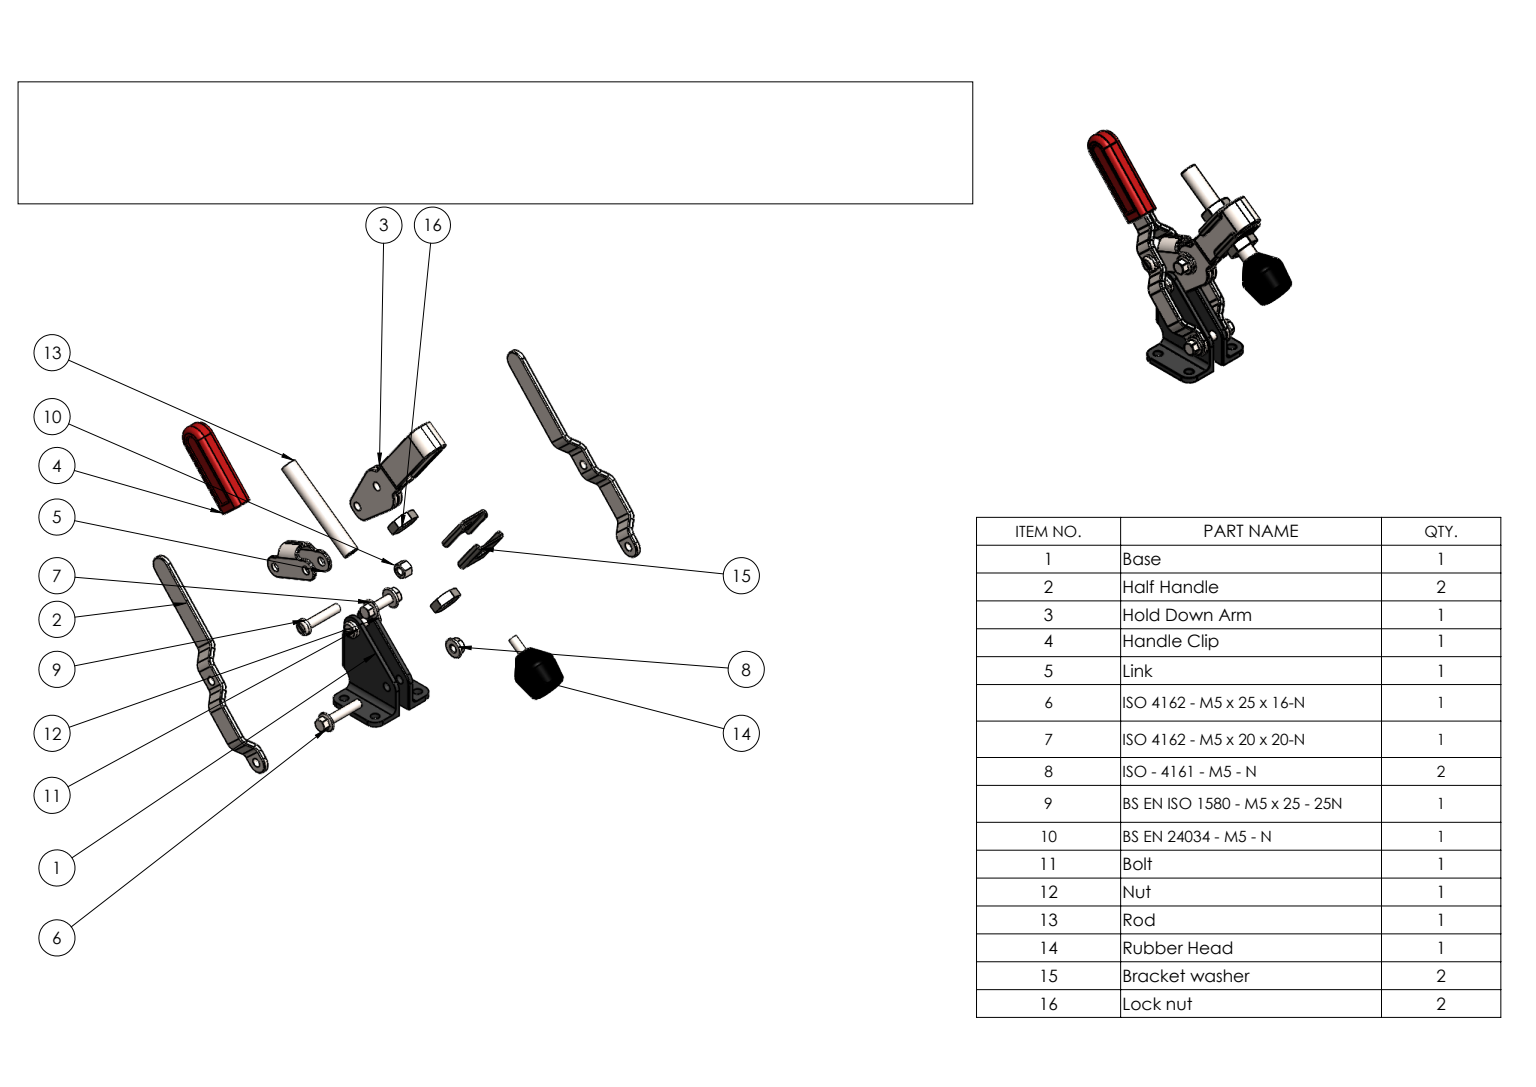
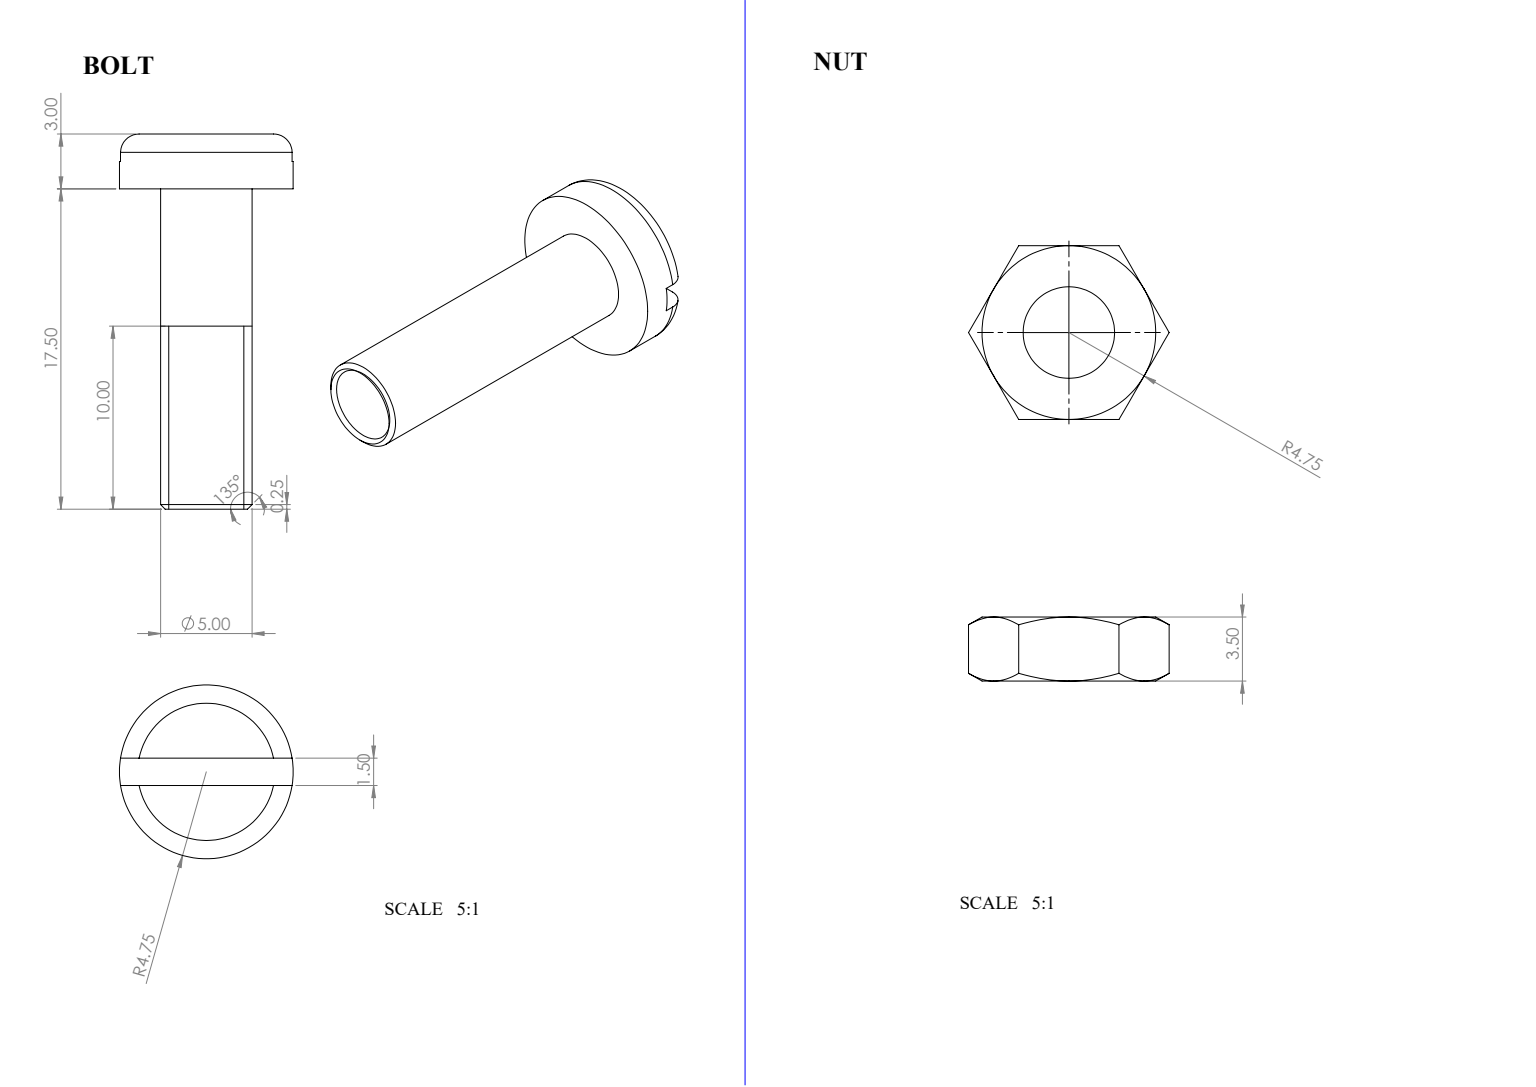
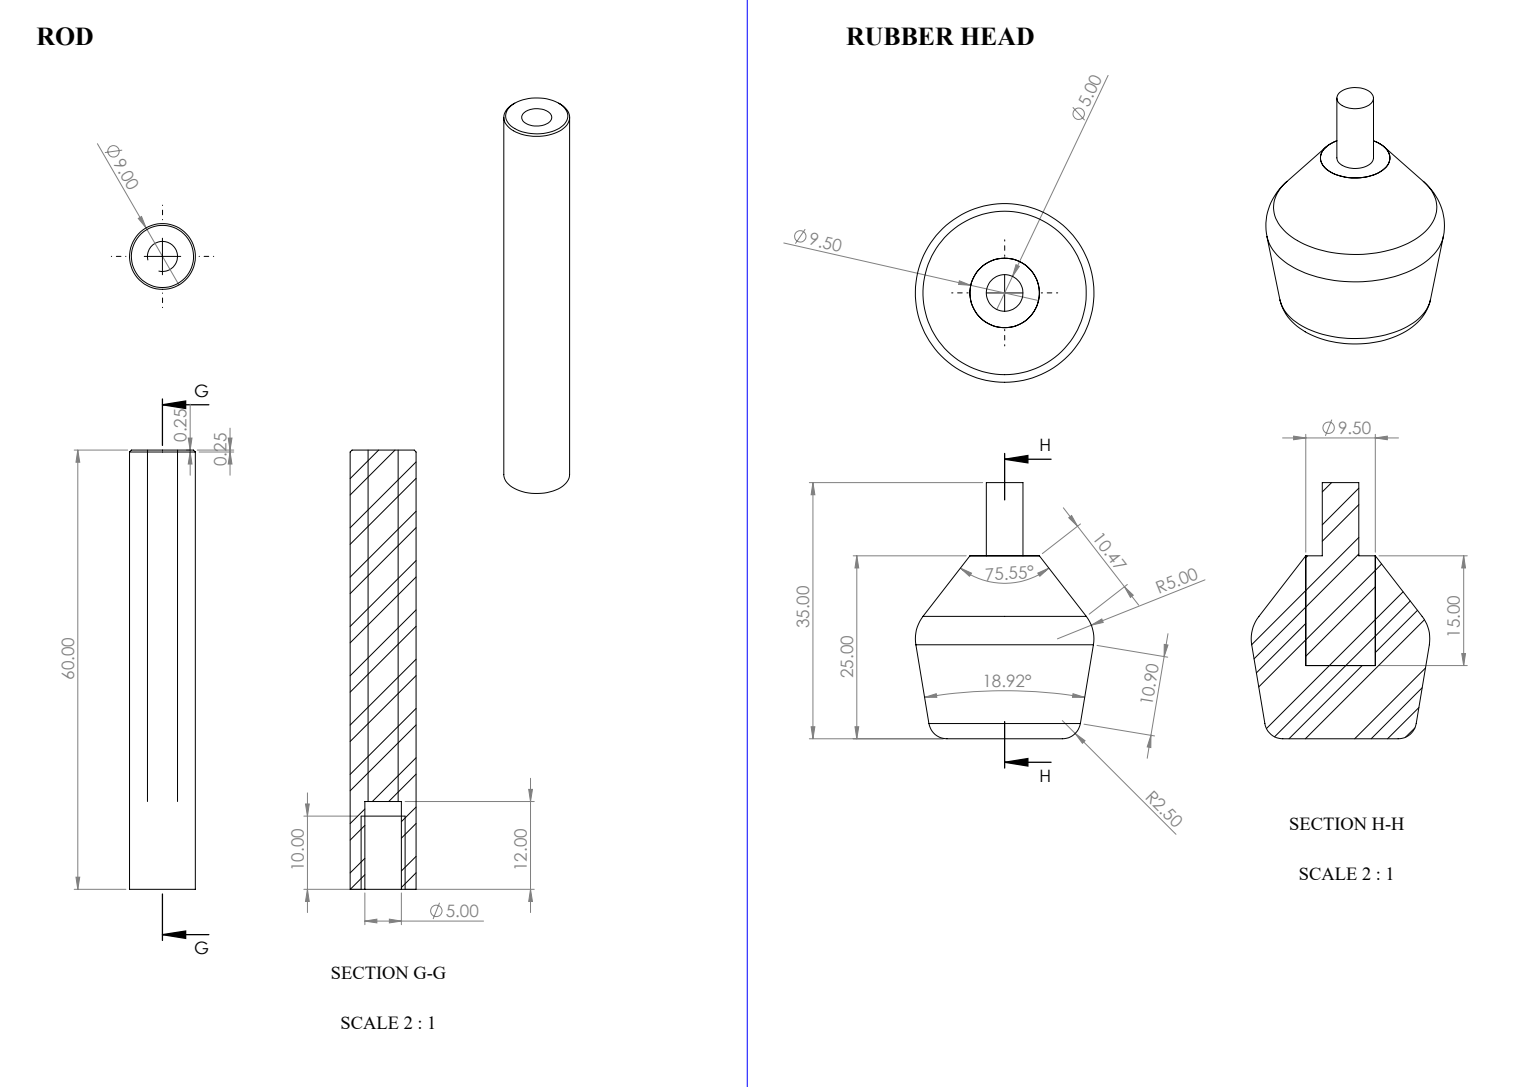
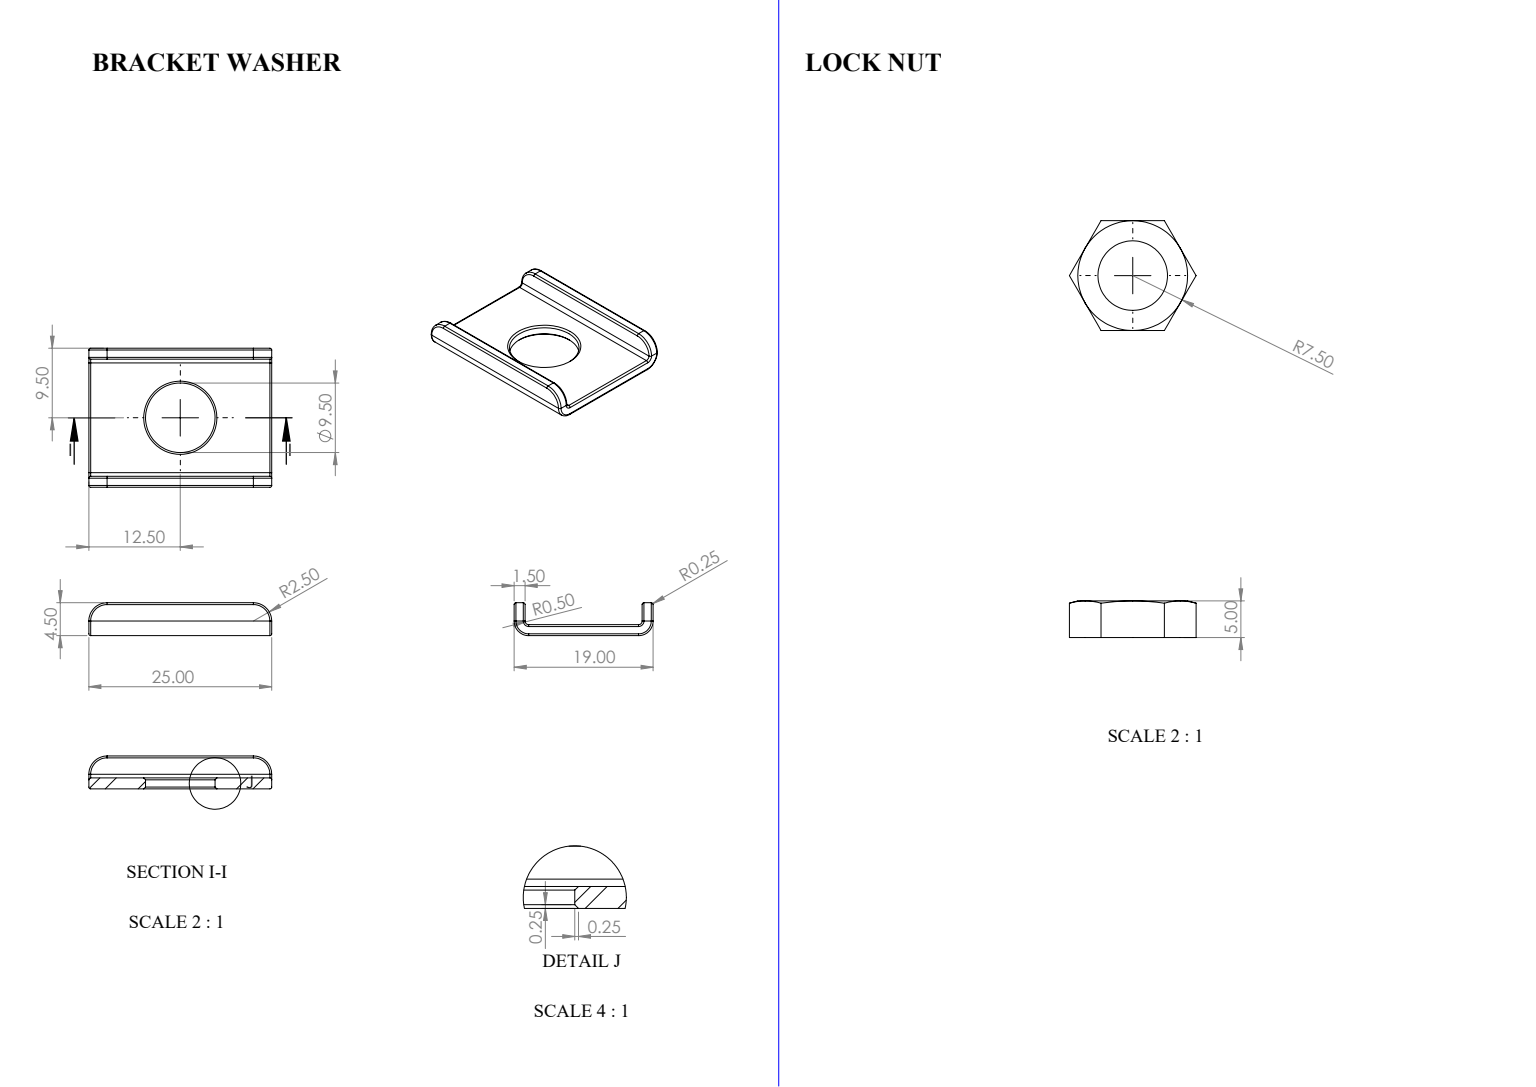
ISO-10303-21;
HEADER;
FILE_DESCRIPTION (('STEP AP214'),
    '1' );
FILE_NAME ('MAS-693',
    '2026-10-06T08:09:25',
    ( '' ),
    ( '' ),
    'SwSTEP 2.0',
    'SolidWorks 2021',
    '' );
FILE_SCHEMA (( 'AUTOMOTIVE_DESIGN' ));
ENDSEC;

DATA;
#1 = CARTESIAN_POINT ( 'NONE',  ( 2.099999999999999645, 0.000000000000000000, -5.294516984716112873 ) ) ;
#2 = DIRECTION ( 'NONE',  ( -0.000000000000000000, 1.000000000000000000, -0.000000000000000000 ) ) ;
#3 = ORIENTED_EDGE ( 'NONE', *, *, #3053, .T. ) ;
#4 = ORIENTED_EDGE ( 'NONE', *, *, #13581, .T. ) ;
#5 = CARTESIAN_POINT ( 'NONE',  ( -4.711587335153455847, 35.99999999900384751, -25.94668155291150313 ) ) ;
#6 = VERTEX_POINT ( 'NONE', #15550 ) ;
#7 = AXIS2_PLACEMENT_3D ( 'NONE', #12336, #20843, #10124 ) ;
#8 = DIRECTION ( 'NONE',  ( 1.000000000000000000, 2.220446049250314560E-16, 0.000000000000000000 ) ) ;
#9 = CARTESIAN_POINT ( 'NONE',  ( -55.05572809000119605, -2.700000000000125855, -7.500000000000062172 ) ) ;
#10 = PRODUCT_DEFINITION_FORMATION_WITH_SPECIFIED_SOURCE ( 'ANY', '', #19447, .NOT_KNOWN. ) ;
#11 = DIRECTION ( 'NONE',  ( 1.000000000000000000, -4.190823558986610327E-31, 1.733449886265890494E-32 ) ) ;
#12 = PRODUCT_RELATED_PRODUCT_CATEGORY ( 'part', '', ( #23234 ) ) ;
#13 = CARTESIAN_POINT ( 'NONE',  ( 2.775557561562891351E-14, 10.75000000000000000, -10.43301270189220276 ) ) ;
#14 = EDGE_LOOP ( 'NONE', ( #2614, #10567, #22264, #5073 ) ) ;
#15 = CYLINDRICAL_SURFACE ( 'NONE', #19275, 7.000000000000075495 ) ;
#16 = FACE_OUTER_BOUND ( 'NONE', #19834, .T. ) ;
#17 = CARTESIAN_POINT ( 'NONE',  ( 2.775557561562891351E-14, 11.00000000000000000, -6.499999999999950262 ) ) ;
#18 = DIRECTION ( 'NONE',  ( -1.000000000000000000, 1.424116703980815236E-16, 2.931272055834072749E-32 ) ) ;
#19 = EDGE_CURVE ( 'NONE', #13411, #2264, #4371, .T. ) ;
#20 = CARTESIAN_POINT ( 'NONE',  ( -47.82842712474649716, 4.371572875253824542, 8.000000000000021316 ) ) ;
#21 = CARTESIAN_POINT ( 'NONE',  ( 8.498922697886333921, -1.509195795641886439, 6.997949321565420711 ) ) ;
#22 = LINE ( 'NONE', #7190, #18522 ) ;
#23 = CARTESIAN_POINT ( 'NONE',  ( 2.775557561562891351E-14, 8.000000000000003553, -6.499999999999950262 ) ) ;
#24 = DIRECTION ( 'NONE',  ( -5.551115123125782702E-16, -1.201780285297635172E-31, 1.000000000000000000 ) ) ;
#25 = CARTESIAN_POINT ( 'NONE',  ( 0.3126073911696447549, -2.020725942163688504, 3.499999999999997780 ) ) ;
#26 = AXIS2_PLACEMENT_3D ( 'NONE', #18449, #2330, #9512 ) ;
#27 = CARTESIAN_POINT ( 'NONE',  ( -50.65685424949274562, -3.200000000000091660, 7.500000000000076383 ) ) ;
#28 = ORIENTED_EDGE ( 'NONE', *, *, #13424, .F. ) ;
#29 = ITEM_DEFINED_TRANSFORMATION ( 'NONE', 'NONE', #18040,  #22115 ) ;
#31 = EDGE_LOOP ( 'NONE', ( #17480, #19110, #8752, #782 ) ) ;
#30 = ORIENTED_EDGE ( 'NONE', *, *, #19301, .F. ) ;
#32 = EDGE_CURVE ( 'NONE', #19371, #4871, #12562, .T. ) ;
#33 = ORIENTED_EDGE ( 'NONE', *, *, #6783, .T. ) ;
#35 = ORIENTED_EDGE ( 'NONE', *, *, #12081, .T. ) ;
#34 = ORIENTED_EDGE ( 'NONE', *, *, #10798, .T. ) ;
#36 = CARTESIAN_POINT ( 'NONE',  ( 0.000000000000000000, 0.000000000000000000, -5.600000000000000533 ) ) ;
#37 = DIRECTION ( 'NONE',  ( 1.000000000000000000, 4.252453317207022018E-31, -5.551115123125818447E-17 ) ) ;
#38 = ADVANCED_FACE ( 'NONE', ( #17307 ), #9922, .T. ) ;
#39 = CARTESIAN_POINT ( 'NONE',  ( 7.263517083688578069, -11.72058614530574694, 7.724990489865656507 ) ) ;
#40 = CIRCLE ( 'NONE', #19182, 2.550000000000002043 ) ;
#41 = CARTESIAN_POINT ( 'NONE',  ( -6.999999999999978684, -10.98142396999974046, 8.916666666666724694 ) ) ;
#42 = CARTESIAN_POINT ( 'NONE',  ( 0.2500000000000071609, 2.000000000000001776, -0.2500000000000002220 ) ) ;
#43 = CARTESIAN_POINT ( 'NONE',  ( 7.909386411297032460, -13.36290293203342650, 7.731447622712527057 ) ) ;
#44 = EDGE_CURVE ( 'NONE', #15578, #10139, #5040, .T. ) ;
#45 = DIRECTION ( 'NONE',  ( 5.916456789157585037E-31, -0.4999999999999997224, 0.8660254037844388186 ) ) ;
#46 = FACE_OUTER_BOUND ( 'NONE', #18970, .T. ) ;
#47 = CARTESIAN_POINT ( 'NONE',  ( 12.84999999999997300, -1.999999999999998224, -2.550000000000000711 ) ) ;
#48 = DIRECTION ( 'NONE',  ( -2.168404344971017743E-16, -1.000000000000000000, 6.982962677686261977E-15 ) ) ;
#49 = DIRECTION ( 'NONE',  ( 0.000000000000000000, 0.000000000000000000, 1.000000000000000000 ) ) ;
#50 = EDGE_CURVE ( 'NONE', #20148, #6938, #11790, .T. ) ;
#51 = CYLINDRICAL_SURFACE ( 'NONE', #1797, 0.4999999999999995559 ) ;
#52 = EDGE_CURVE ( 'NONE', #21352, #10482, #865, .T. ) ;
#53 = CARTESIAN_POINT ( 'NONE',  ( 5.773502691896164052, 4.999999999999978684, 4.999999999999978684 ) ) ;
#54 = CARTESIAN_POINT ( 'NONE',  ( 0.000000000000000000, 3.031088913245528982, -1.750000000000001554 ) ) ;
#55 = EDGE_CURVE ( 'NONE', #3237, #11583, #13792, .T. ) ;
#56 = EDGE_LOOP ( 'NONE', ( #13558, #11700, #20158, #8031 ) ) ;
#57 = TOROIDAL_SURFACE ( 'NONE', #21466, 6.000000000000000000, 0.5000000000000000000 ) ;
#59 = ORIENTED_EDGE ( 'NONE', *, *, #18406, .T. ) ;
#58 = ORIENTED_EDGE ( 'NONE', *, *, #7145, .T. ) ;
#60 = ORIENTED_EDGE ( 'NONE', *, *, #16971, .F. ) ;
#62 = ORIENTED_EDGE ( 'NONE', *, *, #144, .F. ) ;
#61 = ORIENTED_EDGE ( 'NONE', *, *, #623, .T. ) ;
#63 = ORIENTED_EDGE ( 'NONE', *, *, #11679, .F. ) ;
#64 = EDGE_CURVE ( 'NONE', #19657, #547, #12184, .T. ) ;
#65 = ORIENTED_EDGE ( 'NONE', *, *, #2173, .F. ) ;
#66 = ORIENTED_EDGE ( 'NONE', *, *, #4342, .F. ) ;
#67 = EDGE_CURVE ( 'NONE', #21664, #15682, #5815, .T. ) ;
#68 = CARTESIAN_POINT ( 'NONE',  ( 12.49999999999995914, 2.775557561562891982E-14, -4.500000000000002665 ) ) ;
#69 = ADVANCED_FACE ( 'NONE', ( #20975 ), #1306, .T. ) ;
#70 = CARTESIAN_POINT ( 'NONE',  ( -42.54314575050785407, -5.300000000000037126, -7.500000000000007105 ) ) ;
#71 = DIRECTION ( 'NONE',  ( -1.000000000000000000, -5.598259082250514647E-17, -3.330669073875432643E-16 ) ) ;
#72 = FACE_OUTER_BOUND ( 'NONE', #12536, .T. ) ;
#73 = DIRECTION ( 'NONE',  ( -0.9878135252003118483, -1.627025617018325989E-30, 0.1556420233463095271 ) ) ;
#74 = CARTESIAN_POINT ( 'NONE',  ( 119.5756419024615838, -4.500000000000059508, -6.499999999999970690 ) ) ;
#75 = AXIS2_PLACEMENT_3D ( 'NONE', #705, #21992, #9988 ) ;
#76 = VECTOR ( 'NONE', #7557, 1000.000000000000000 ) ;
#77 = CARTESIAN_POINT ( 'NONE',  ( -2.836893136758718903, -3.208949435745849676, -3.505054077164919235 ) ) ;
#78 = EDGE_CURVE ( 'NONE', #1099, #6825, #11430, .T. ) ;
#79 = CARTESIAN_POINT ( 'NONE',  ( 2.775557561562891351E-14, 0.000000000000000000, -6.000000000000019540 ) ) ;
#80 = CARTESIAN_POINT ( 'NONE',  ( 3.806834918298653392, 3.031088913245603589, -1.750000000000057065 ) ) ;
#81 = EDGE_CURVE ( 'NONE', #17539, #20156, #20469, .T. ) ;
#82 = CYLINDRICAL_SURFACE ( 'NONE', #15543, 0.4999999999999995559 ) ;
#83 = PLANE ( 'NONE',  #17902 ) ;
#84 = VERTEX_POINT ( 'NONE', #16838 ) ;
#85 =( NAMED_UNIT ( * ) PLANE_ANGLE_UNIT ( ) SI_UNIT ( $, .RADIAN. ) );
#86 = DIRECTION ( 'NONE',  ( 8.438582421954109416E-32, 0.000000000000000000, 1.000000000000000000 ) ) ;
#88 = ORIENTED_EDGE ( 'NONE', *, *, #2993, .T. ) ;
#87 = ORIENTED_EDGE ( 'NONE', *, *, #1268, .T. ) ;
#89 = ORIENTED_EDGE ( 'NONE', *, *, #7270, .T. ) ;
#90 = CIRCLE ( 'NONE', #20736, 0.5000000000000004441 ) ;
#91 = CIRCLE ( 'NONE', #20737, 0.4999999999999994449 ) ;
#92 = ORIENTED_EDGE ( 'NONE', *, *, #20127, .T. ) ;
#93 = VERTEX_POINT ( 'NONE', #8036 ) ;
#94 = CARTESIAN_POINT ( 'NONE',  ( 7.499999999999978684, 1.734723475976807094E-14, 9.249999999999980460 ) ) ;
#95 = CARTESIAN_POINT ( 'NONE',  ( 5.213674118230995802, -0.7499999999999382716, -1.500000000000001332 ) ) ;
#96 = DIRECTION ( 'NONE',  ( -4.336808689942052446E-15, -1.000000000000000000, -3.574525976782710619E-31 ) ) ;
#97 = CARTESIAN_POINT ( 'NONE',  ( 3.973514160553469843, -2.741076955031381157, -2.383932505289878101 ) ) ;
#98 = DIRECTION ( 'NONE',  ( 0.000000000000000000, -1.000000000000000000, 0.000000000000000000 ) ) ;
#99 = DIRECTION ( 'NONE',  ( -1.000000000000000000, -2.220446049250313081E-16, 0.000000000000000000 ) ) ;
#100 = CARTESIAN_POINT ( 'NONE',  ( -6.938893903907228378E-15, -22.91099746826335348, -1.387778780781445676E-14 ) ) ;
#101 = ADVANCED_FACE ( 'NONE', ( #18737 ), #22509, .T. ) ;
#102 = DIRECTION ( 'NONE',  ( 0.000000000000000000, 0.000000000000000000, 1.000000000000000000 ) ) ;
#103 = DIRECTION ( 'NONE',  ( -2.220446049250313081E-16, 1.000000000000000000, -7.025792437124636392E-31 ) ) ;
#104 = CARTESIAN_POINT ( 'NONE',  ( 37.00000000000030553, 10.74999999999998579, -10.43301270189227559 ) ) ;
#105 = LINE ( 'NONE', #16189, #2754 ) ;
#106 = CARTESIAN_POINT ( 'NONE',  ( -2.725741868434905513, 3.045094352034741547, -3.220599429844064332 ) ) ;
#107 = AXIS2_PLACEMENT_3D ( 'NONE', #10783, #22922, #6797 ) ;
#108 = EDGE_CURVE ( 'NONE', #6044, #8580, #6954, .T. ) ;
#109 = FACE_OUTER_BOUND ( 'NONE', #9678, .T. ) ;
#110 = DIRECTION ( 'NONE',  ( 3.032184104443271834E-30, 1.000000000000000000, 4.437342591868167759E-31 ) ) ;
#111 = ORIENTED_EDGE ( 'NONE', *, *, #7820, .T. ) ;
#112 = ORIENTED_EDGE ( 'NONE', *, *, #14818, .T. ) ;
#113 = DIRECTION ( 'NONE',  ( -0.7313537016191756779, 0.6819983600624930364, -4.478224685260177339E-16 ) ) ;
#114 = ORIENTED_EDGE ( 'NONE', *, *, #778, .F. ) ;
#115 = CIRCLE ( 'NONE', #13253, 5.200000000000008171 ) ;
#116 = CARTESIAN_POINT ( 'NONE',  ( 2.712762565639641021, -3.052587955997488223, -3.430618716626634424 ) ) ;
#117 = CONICAL_SURFACE ( 'NONE', #18527, 7.499999999999998224, 1.308996938995750092 ) ;
#118 = AXIS2_PLACEMENT_3D ( 'NONE', #12279, #12167, #17943 ) ;
#119 = DIRECTION ( 'NONE',  ( -1.000000000000000000, -1.479114197289388027E-30, 2.013525853228518840E-32 ) ) ;
#120 = FACE_OUTER_BOUND ( 'NONE', #16147, .T. ) ;
#121 = AXIS2_PLACEMENT_3D ( 'NONE', #9275, #21645, #19978 ) ;
#122 = CARTESIAN_POINT ( 'NONE',  ( -92.25000000000058265, -8.981013850637800498E-14, -2.000000000000001776 ) ) ;
#123 = ORIENTED_EDGE ( 'NONE', *, *, #8630, .F. ) ;
#124 = LINE ( 'NONE', #8704, #11013 ) ;
#125 = DIRECTION ( 'NONE',  ( -3.885780586188016830E-16, -4.437342591868156373E-31, 1.000000000000000000 ) ) ;
#126 = DIRECTION ( 'NONE',  ( 2.013525853228507892E-32, 6.902532920683810383E-31, -1.000000000000000000 ) ) ;
#127 = CARTESIAN_POINT ( 'NONE',  ( 7.499999999999978684, -2.645898033750298417, 9.250000000000021316 ) ) ;
#128 = CARTESIAN_POINT ( 'NONE',  ( -89.70000000000064233, 2.700000000000056577, -2.000000000000001776 ) ) ;
#129 = CARTESIAN_POINT ( 'NONE',  ( 8.697224362268009656, -1.999999999999984013, 6.249999999999998224 ) ) ;
#130 = CARTESIAN_POINT ( 'NONE',  ( 4.071447262713884463, 2.020725942163639655, -3.499999999999996003 ) ) ;
#131 = CYLINDRICAL_SURFACE ( 'NONE', #16076, 2.000000000000015543 ) ;
#132 = CARTESIAN_POINT ( 'NONE',  ( 25.00000000000000355, 2.000000000000001776, -1.250000000000004663 ) ) ;
#133 = AXIS2_PLACEMENT_3D ( 'NONE', #13173, #11168, #18350 ) ;
#134 = DIRECTION ( 'NONE',  ( 1.000000000000000000, 0.000000000000000000, 0.000000000000000000 ) ) ;
#135 = CIRCLE ( 'NONE', #13271, 0.5000000000000004441 ) ;
#136 = AXIS2_PLACEMENT_3D ( 'NONE', #2395, #9803, #3063 ) ;
#137 = AXIS2_PLACEMENT_3D ( 'NONE', #8620, #22982, #10500 ) ;
#138 = VERTEX_POINT ( 'NONE', #8274 ) ;
#139 = AXIS2_PLACEMENT_3D ( 'NONE', #3664, #23097, #6847 ) ;
#140 =( GEOMETRIC_REPRESENTATION_CONTEXT ( 3 ) GLOBAL_UNCERTAINTY_ASSIGNED_CONTEXT ( ( #4137 ) ) GLOBAL_UNIT_ASSIGNED_CONTEXT ( ( #21562, #16354, #5447 ) ) REPRESENTATION_CONTEXT ( 'NONE', 'WORKASPACE' ) );
#141 = APPLICATION_PROTOCOL_DEFINITION ( 'draft international standard', 'automotive_design', 1998, #14336 ) ;
#143 = EDGE_LOOP ( 'NONE', ( #667, #18574, #6068, #5287 ) ) ;
#142 = ORIENTED_EDGE ( 'NONE', *, *, #22317, .T. ) ;
#144 = EDGE_CURVE ( 'NONE', #13324, #19219, #20095, .T. ) ;
#145 = VERTEX_POINT ( 'NONE', #20516 ) ;
#147 = ORIENTED_EDGE ( 'NONE', *, *, #4920, .T. ) ;
#146 = ORIENTED_EDGE ( 'NONE', *, *, #6538, .T. ) ;
#148 = CARTESIAN_POINT ( 'NONE',  ( 119.5756419024615269, -11.00000000000006573, 6.000000000000081712 ) ) ;
#149 = CARTESIAN_POINT ( 'NONE',  ( 7.554637128289398262, -0.1201405311246625390, 7.453047528892632556 ) ) ;
#150 = CARTESIAN_POINT ( 'NONE',  ( 8.723547172042144027, -11.98401194435536432, 6.817515300135809753 ) ) ;
#151 = AXIS2_PLACEMENT_3D ( 'NONE', #11597, #19127, #20797 ) ;
#152 = AXIS2_PLACEMENT_3D ( 'NONE', #5181, #12341, #17885 ) ;
#153 = CARTESIAN_POINT ( 'NONE',  ( 7.000000000000006217, -11.35410196624971491, 9.250000000000008882 ) ) ;
#154 = TOROIDAL_SURFACE ( 'NONE', #10279, 5.500000000000007994, 0.5000000000000000000 ) ;
#155 = CARTESIAN_POINT ( 'NONE',  ( -55.25320565519145788, 0.5000000000000905942, 10.00000000000009237 ) ) ;
#156 = VECTOR ( 'NONE', #8671, 1000.000000000000227 ) ;
#157 = CARTESIAN_POINT ( 'NONE',  ( 4.560256354962182179, -0.7499999999999382716, -2.508007965330665723 ) ) ;
#158 = AXIS2_PLACEMENT_3D ( 'NONE', #22123, #20356, #13067 ) ;
#159 = SURFACE_STYLE_FILL_AREA ( #10728 ) ;
#160 = DIRECTION ( 'NONE',  ( 1.000000000000000000, 2.220446049250313081E-16, -3.656342123407315983E-48 ) ) ;
#161 = CARTESIAN_POINT ( 'NONE',  ( -12.85000000000004228, -0.5000000000000004441, -6.249999999999977796 ) ) ;
#162 = DIRECTION ( 'NONE',  ( 2.172745813409349776E-17, -1.000000000000000000, 1.309377075419428048E-16 ) ) ;
#163 = CARTESIAN_POINT ( 'NONE',  ( 4.346882592290810088, -1.739972214219157598, -1.970978495615625325 ) ) ;
#164 = DIRECTION ( 'NONE',  ( -9.121204216617949000E-31, -1.000000000000000000, 6.982962677686261977E-15 ) ) ;
#165 = FACE_OUTER_BOUND ( 'NONE', #636, .T. ) ;
#166 = DIRECTION ( 'NONE',  ( -0.7071067811865475727, -0.7071067811865475727, 0.000000000000000000 ) ) ;
#167 = CARTESIAN_POINT ( 'NONE',  ( 8.204963667274160599, -0.08625821904936173401, 7.312308861538857840 ) ) ;
#168 = ORIENTED_EDGE ( 'NONE', *, *, #3680, .T. ) ;
#169 = ADVANCED_FACE ( 'NONE', ( #20745 ), #4609, .T. ) ;
#170 = AXIS2_PLACEMENT_3D ( 'NONE', #22281, #4382, #9585 ) ;
#172 = VERTEX_POINT ( 'NONE', #11900 ) ;
#171 = ORIENTED_EDGE ( 'NONE', *, *, #19907, .F. ) ;
#173 = VECTOR ( 'NONE', #16606, 1000.000000000000000 ) ;
#174 = EDGE_CURVE ( 'NONE', #11003, #22641, #9065, .T. ) ;
#175 = ORIENTED_EDGE ( 'NONE', *, *, #6794, .T. ) ;
#177 = EDGE_LOOP ( 'NONE', ( #17810, #15690, #3320, #5048, #142 ) ) ;
#176 = EDGE_LOOP ( 'NONE', ( #1008, #14393, #11718, #4703 ) ) ;
#178 = VERTEX_POINT ( 'NONE', #19086 ) ;
#179 = LINE ( 'NONE', #15827, #9133 ) ;
#180 = VERTEX_POINT ( 'NONE', #3214 ) ;
#181 = ORIENTED_EDGE ( 'NONE', *, *, #18463, .F. ) ;
#182 = DIRECTION ( 'NONE',  ( -0.7071067811865435759, 2.143845182814170115E-16, -0.7071067811865514585 ) ) ;
#183 = EDGE_CURVE ( 'NONE', #9368, #15940, #10370, .T. ) ;
#184 = EDGE_CURVE ( 'NONE', #21240, #19103, #1689, .T. ) ;
#185 = FACE_OUTER_BOUND ( 'NONE', #9063, .T. ) ;
#186 = EDGE_CURVE ( 'NONE', #15772, #2089, #3930, .T. ) ;
#187 = CARTESIAN_POINT ( 'NONE',  ( 24.99999999999998934, 1.500000000000001332, -2.000000000000005329 ) ) ;
#188 = CARTESIAN_POINT ( 'NONE',  ( 0.1388410611046271836, 2.351840044243041827, -2.926493552096059769 ) ) ;
#189 = FACE_OUTER_BOUND ( 'NONE', #10029, .T. ) ;
#190 = CARTESIAN_POINT ( 'NONE',  ( -42.54314575050778302, -8.000000000000021316, 7.500000000000034639 ) ) ;
#191 = STYLED_ITEM ( 'NONE', ( #6397 ), #12837 ) ;
#192 = DIRECTION ( 'NONE',  ( 5.551115123125782702E-16, 1.201780285297635172E-31, -1.000000000000000000 ) ) ;
#193 = CARTESIAN_POINT ( 'NONE',  ( -12.84999999999999964, -1.500000000000001332, 5.750000000000005329 ) ) ;
#194 = LINE ( 'NONE', #770, #19044 ) ;
#195 = VERTEX_POINT ( 'NONE', #8969 ) ;
#196 = EDGE_CURVE ( 'NONE', #1099, #11721, #4693, .T. ) ;
#197 = EDGE_CURVE ( 'NONE', #5639, #7574, #985, .T. ) ;
#198 = FACE_OUTER_BOUND ( 'NONE', #17875, .T. ) ;
#200 = ORIENTED_EDGE ( 'NONE', *, *, #2322, .T. ) ;
#199 = ORIENTED_EDGE ( 'NONE', *, *, #4642, .F. ) ;
#201 = AXIS2_PLACEMENT_3D ( 'NONE', #19066, #17054, #16931 ) ;
#202 = ADVANCED_BREP_SHAPE_REPRESENTATION ( '', ( #21257, #21014, #22115 ), #20270 ) ;
#203 = ORIENTED_EDGE ( 'NONE', *, *, #5369, .T. ) ;
#204 = EDGE_CURVE ( 'NONE', #21236, #14256, #17064, .T. ) ;
#205 = EDGE_LOOP ( 'NONE', ( #9340, #20187 ) ) ;
#206 = FACE_OUTER_BOUND ( 'NONE', #13645, .T. ) ;
#207 = ADVANCED_FACE ( 'NONE', ( #3092, #23213, #8851 ), #10257, .T. ) ;
#208 = EDGE_CURVE ( 'NONE', #21919, #22681, #22973, .T. ) ;
#209 = CARTESIAN_POINT ( 'NONE',  ( 4.050823680195219545, 2.400527758044904925, 2.978030508226147344 ) ) ;
#210 = LINE ( 'NONE', #7721, #18126 ) ;
#211 = DIRECTION ( 'NONE',  ( 1.454462294001240516E-30, 1.000000000000000000, 0.000000000000000000 ) ) ;
#212 = DIRECTION ( 'NONE',  ( -2.172745813409349776E-17, 1.000000000000000000, -1.309377075419428048E-16 ) ) ;
#213 = DIRECTION ( 'NONE',  ( -2.168404344971017743E-16, -1.000000000000000000, 6.982962677686261977E-15 ) ) ;
#214 = B_SPLINE_CURVE_WITH_KNOTS ( 'NONE', 3,
 ( #18119, #8839, #16105, #19776, #9183, #244, #12819, #19998 ),
 .UNSPECIFIED., .F., .F.,
 ( 4, 2, 2, 4 ),
 ( 0.005725059856848683376, 0.006314084072593680388, 0.006903108288338678268, 0.008081156719828673160 ),
 .UNSPECIFIED. ) ;
#215 = CARTESIAN_POINT ( 'NONE',  ( -8.195710046796538251, -2.011959044857179357, 6.570882465138005557 ) ) ;
#216 = DIRECTION ( 'NONE',  ( 1.000000000000000000, 5.598259082250514647E-17, 3.330669073875432643E-16 ) ) ;
#217 = EDGE_CURVE ( 'NONE', #19662, #17819, #14141, .T. ) ;
#218 = AXIS2_PLACEMENT_3D ( 'NONE', #14602, #2245, #20126 ) ;
#219 = CARTESIAN_POINT ( 'NONE',  ( 10.49999999999999467, -14.00000000000000888, 9.250000000000063949 ) ) ;
#220 = DIRECTION ( 'NONE',  ( -1.000000000000000000, -2.220446049250314067E-16, 5.825996348268307008E-33 ) ) ;
#221 = CARTESIAN_POINT ( 'NONE',  ( 37.36637401601599606, 0.3137297356303613283, -10.36637401601559105 ) ) ;
#222 = ADVANCED_FACE ( 'NONE', ( #21089 ), #12579, .F. ) ;
#223 = DIRECTION ( 'NONE',  ( -1.066786462891689527E-26, -6.656013887802287108E-31, -1.000000000000000000 ) ) ;
#224 = CARTESIAN_POINT ( 'NONE',  ( -10.49999999999999467, -1.500000000000001332, 5.750000000000005329 ) ) ;
#225 = ORIENTED_EDGE ( 'NONE', *, *, #17691, .F. ) ;
#226 = VERTEX_POINT ( 'NONE', #7205 ) ;
#227 = EDGE_CURVE ( 'NONE', #18640, #22996, #18594, .T. ) ;
#228 = CARTESIAN_POINT ( 'NONE',  ( -55.05572809000122447, -2.700000000000125855, -10.00000000000006395 ) ) ;
#229 = ORIENTED_EDGE ( 'NONE', *, *, #14979, .F. ) ;
#230 = APPLICATION_CONTEXT ( 'automotive_design' ) ;
#231 = CARTESIAN_POINT ( 'NONE',  ( 54.42435809754113052, -4.000000000000003553, -6.000000000000012434 ) ) ;
#232 = LINE ( 'NONE', #4899, #1007 ) ;
#233 = CARTESIAN_POINT ( 'NONE',  ( 4.180231891692635315, -2.049421325483237410, -3.591231015387320813 ) ) ;
#234 = DIRECTION ( 'NONE',  ( 0.000000000000000000, 0.000000000000000000, 1.000000000000000000 ) ) ;
#235 = VERTEX_POINT ( 'NONE', #17541 ) ;
#236 = CIRCLE ( 'NONE', #19764, 2.999999999999995559 ) ;
#237 = DIRECTION ( 'NONE',  ( 1.333893503340774882E-15, 2.778352770573747380E-17, 1.000000000000000000 ) ) ;
#238 = CARTESIAN_POINT ( 'NONE',  ( 0.3126073911696378160, 2.020725942163612121, 3.499999999999975131 ) ) ;
#239 = DIRECTION ( 'NONE',  ( -1.000000000000000000, 0.000000000000000000, -3.330669073875408978E-16 ) ) ;
#240 = DIRECTION ( 'NONE',  ( -2.013525853228508439E-32, -6.779273404243028164E-31, 1.000000000000000000 ) ) ;
#241 = CARTESIAN_POINT ( 'NONE',  ( 8.510464245293309915, -13.49280278100692243, 6.988717072694059063 ) ) ;
#242 = DIRECTION ( 'NONE',  ( 1.000000000000000000, 1.479114197289387852E-30, -2.013525853228518840E-32 ) ) ;
#243 = CARTESIAN_POINT ( 'NONE',  ( 3.972066048304788932, 2.740530939476398142, -2.384802634787798414 ) ) ;
#244 = CARTESIAN_POINT ( 'NONE',  ( 3.999999999999940048, 1.563622288139227656, -0.2253451193527943042 ) ) ;
#245 = PRODUCT_CONTEXT ( 'NONE', #18364, 'mechanical' ) ;
#247 = ORIENTED_EDGE ( 'NONE', *, *, #13683, .T. ) ;
#246 = ORIENTED_EDGE ( 'NONE', *, *, #14573, .F. ) ;
#248 = ADVANCED_FACE ( 'NONE', ( #1437 ), #12950, .T. ) ;
#249 = VECTOR ( 'NONE', #5863, 1000.000000000000000 ) ;
#251 = ORIENTED_EDGE ( 'NONE', *, *, #16111, .T. ) ;
#250 = ORIENTED_EDGE ( 'NONE', *, *, #16395, .F. ) ;
#252 = CARTESIAN_POINT ( 'NONE',  ( -4.330127018922255822, -9.714451465470119729E-14, 7.499999999999985789 ) ) ;
#253 = ADVANCED_FACE ( 'NONE', ( #8611 ), #5204, .T. ) ;
#254 = CARTESIAN_POINT ( 'NONE',  ( 37.09721192197999073, 0.1772999597157984553, -2.518381337117822305 ) ) ;
#255 = CARTESIAN_POINT ( 'NONE',  ( 7.000000000000001776, -10.98142396999974935, 8.916666666666673180 ) ) ;
#256 = DIRECTION ( 'NONE',  ( 0.000000000000000000, -1.000000000000000000, 0.000000000000000000 ) ) ;
#257 = FACE_OUTER_BOUND ( 'NONE', #3493, .T. ) ;
#258 = FACE_OUTER_BOUND ( 'NONE', #543, .T. ) ;
#259 = FACE_OUTER_BOUND ( 'NONE', #10192, .T. ) ;
#260 = CARTESIAN_POINT ( 'NONE',  ( 6.000000000291855429, -0.5000000009961480529, -5.999999999999998224 ) ) ;
#261 = DIRECTION ( 'NONE',  ( 0.000000000000000000, 0.000000000000000000, -1.000000000000000000 ) ) ;
#262 = LINE ( 'NONE', #18378, #17735 ) ;
#263 = LINE ( 'NONE', #5220, #12168 ) ;
#264 = DIRECTION ( 'NONE',  ( 1.000000000000000000, -4.190823558986610327E-31, 1.733449886265890494E-32 ) ) ;
#265 = CIRCLE ( 'NONE', #18661, 4.500000000000045297 ) ;
#266 = CARTESIAN_POINT ( 'NONE',  ( 1.660531772554329821, -3.660093687634887072, -5.599999999999980105 ) ) ;
#267 = STYLED_ITEM ( 'NONE', ( #8597 ), #21014 ) ;
#268 = CARTESIAN_POINT ( 'NONE',  ( 8.565230440156003766, -1.999999999999984457, 6.320505311736929421 ) ) ;
#269 = CARTESIAN_POINT ( 'NONE',  ( -1.734723475976807094E-14, 1.250000000000001110, -17.00000000000000711 ) ) ;
#270 = CARTESIAN_POINT ( 'NONE',  ( 8.429621201837189659, 1.585786587480479934E-14, 6.425428529984677617 ) ) ;
#271 = ORIENTED_EDGE ( 'NONE', *, *, #15321, .T. ) ;
#272 = VECTOR ( 'NONE', #10209, 1000.000000000000000 ) ;
#274 = ORIENTED_EDGE ( 'NONE', *, *, #19427, .F. ) ;
#273 = VERTEX_POINT ( 'NONE', #8728 ) ;
#275 = B_SPLINE_CURVE_WITH_KNOTS ( 'NONE', 3,
 ( #5062, #11991, #17398, #21068, #10229 ),
 .UNSPECIFIED., .F., .F.,
 ( 4, 1, 4 ),
 ( 0.000000000000000000, 0.002020725942163690073, 0.004041451884327380145 ),
 .UNSPECIFIED. ) ;
#276 = EDGE_LOOP ( 'NONE', ( #1805, #8526, #7103, #1700 ) ) ;
#278 = VERTEX_POINT ( 'NONE', #17790 ) ;
#277 = EDGE_LOOP ( 'NONE', ( #6331, #5519, #19401, #7762 ) ) ;
#279 = CIRCLE ( 'NONE', #13429, 0.5000000000000022204 ) ;
#280 = VERTEX_POINT ( 'NONE', #12363 ) ;
#281 = CARTESIAN_POINT ( 'NONE',  ( 5.484827557301438894, 1.325747111984056037, 0.000000000000000000 ) ) ;
#282 = AXIS2_PLACEMENT_3D ( 'NONE', #9971, #20557, #10084 ) ;
#283 = VERTEX_POINT ( 'NONE', #1674 ) ;
#284 = ORIENTED_EDGE ( 'NONE', *, *, #7716, .T. ) ;
#285 = CARTESIAN_POINT ( 'NONE',  ( 5.600000000000000533, -2.020725942163709377, -3.500000000000010214 ) ) ;
#286 =( NAMED_UNIT ( * ) PLANE_ANGLE_UNIT ( ) SI_UNIT ( $, .RADIAN. ) );
#287 = CARTESIAN_POINT ( 'NONE',  ( 54.42435809754115894, 2.999999999999947153, 6.000000000000136779 ) ) ;
#288 = LINE ( 'NONE', #14177, #16241 ) ;
#289 = PRODUCT_RELATED_PRODUCT_CATEGORY ( 'part', '', ( #2909 ) ) ;
#290 = VECTOR ( 'NONE', #21577, 1000.000000000000000 ) ;
#291 = LINE ( 'NONE', #18180, #3856 ) ;
#292 = DIRECTION ( 'NONE',  ( 0.7071067811865535679, -0.7071067811865414665, 0.000000000000000000 ) ) ;
#293 = CARTESIAN_POINT ( 'NONE',  ( -4.211140560182312420, 2.431303136016568889, -3.745885042887433958 ) ) ;
#294 = PLANE ( 'NONE',  #19723 ) ;
#295 = CIRCLE ( 'NONE', #11546, 0.2500000000000003331 ) ;
#296 = B_SPLINE_CURVE_WITH_KNOTS ( 'NONE', 3,
 ( #9686, #20518, #6167, #6504, #16841 ),
 .UNSPECIFIED., .F., .F.,
 ( 4, 1, 4 ),
 ( 6.992893892674682497E-18, 0.002020725942163693108, 0.004041451884327379278 ),
 .UNSPECIFIED. ) ;
#297 = ADVANCED_FACE ( 'NONE', ( #7100 ), #21448, .T. ) ;
#298 = CARTESIAN_POINT ( 'NONE',  ( -56.87767137932624451, -2.700000000000049472, 8.833333333333415638 ) ) ;
#299 = AXIS2_PLACEMENT_3D ( 'NONE', #21279, #216, #10679 ) ;
#300 = FACE_OUTER_BOUND ( 'NONE', #859, .T. ) ;
#301 = AXIS2_PLACEMENT_3D ( 'NONE', #1691, #21234, #5101 ) ;
#302 = ORIENTED_EDGE ( 'NONE', *, *, #6662, .T. ) ;
#303 = EDGE_CURVE ( 'NONE', #3117, #17483, #12943, .T. ) ;
#304 = B_SPLINE_CURVE_WITH_KNOTS ( 'NONE', 3,
 ( #10582, #16334, #21540, #16095, #19528, #238 ),
 .UNSPECIFIED., .F., .F.,
 ( 4, 2, 4 ),
 ( 0.005852013090620712850, 0.006875955131657994837, 0.007899897172695277692 ),
 .UNSPECIFIED. ) ;
#305 = CARTESIAN_POINT ( 'NONE',  ( -90.55603112840523750, -3.200000000000105427, -7.432974388601742533 ) ) ;
#307 = ORIENTED_EDGE ( 'NONE', *, *, #10358, .F. ) ;
#306 = EDGE_LOOP ( 'NONE', ( #6785, #17565, #11984, #16573 ) ) ;
#308 = ADVANCED_FACE ( 'NONE', ( #18028 ), #17460, .T. ) ;
#309 = ORIENTED_EDGE ( 'NONE', *, *, #10119, .F. ) ;
#310 = AXIS2_PLACEMENT_3D ( 'NONE', #22356, #6236, #2234 ) ;
#311 = ORIENTED_EDGE ( 'NONE', *, *, #11203, .F. ) ;
#312 = AXIS2_PLACEMENT_3D ( 'NONE', #15353, #22544, #11935 ) ;
#313 = ORIENTED_EDGE ( 'NONE', *, *, #17284, .F. ) ;
#314 = ORIENTED_EDGE ( 'NONE', *, *, #20628, .F. ) ;
#315 = CARTESIAN_POINT ( 'NONE',  ( 56.34099918003215635, 0.3656768508095153969, -5.999999999999991118 ) ) ;
#316 = LINE ( 'NONE', #16179, #14360 ) ;
#317 = FACE_OUTER_BOUND ( 'NONE', #6393, .T. ) ;
#318 = EDGE_CURVE ( 'NONE', #5868, #10391, #18968, .T. ) ;
#319 = FACE_OUTER_BOUND ( 'NONE', #20806, .T. ) ;
#320 = CYLINDRICAL_SURFACE ( 'NONE', #22884, 0.2500000000000000000 ) ;
#321 = B_SPLINE_CURVE_WITH_KNOTS ( 'NONE', 3,
 ( #20102, #14913, #7632, #14569 ),
 .UNSPECIFIED., .F., .F.,
 ( 4, 4 ),
 ( 2.380737582390834275E-07, 0.002336974151641598059 ),
 .UNSPECIFIED. ) ;
#322 = AXIS2_PLACEMENT_3D ( 'NONE', #17727, #17856, #12431 ) ;
#323 = FACE_OUTER_BOUND ( 'NONE', #12620, .T. ) ;
#324 = CARTESIAN_POINT ( 'NONE',  ( 88.75737332930587797, -10.52760560296347947, 6.500000000000075495 ) ) ;
#325 = EDGE_CURVE ( 'NONE', #4761, #2725, #5554, .T. ) ;
#326 = DIRECTION ( 'NONE',  ( 1.000000000000000000, 2.220446049250314067E-16, -5.825996348268307008E-33 ) ) ;
#327 = VECTOR ( 'NONE', #12053, 1000.000000000000000 ) ;
#328 = CARTESIAN_POINT ( 'NONE',  ( 2.918498775983380256E-10, 2.999999999003851503, -39.00000000000000000 ) ) ;
#329 = CIRCLE ( 'NONE', #8202, 0.5000000000000004441 ) ;
#330 = AXIS2_PLACEMENT_3D ( 'NONE', #11225, #18403, #21944 ) ;
#331 = DIRECTION ( 'NONE',  ( 9.121204216617949000E-31, 1.000000000000000000, -6.982962677686261977E-15 ) ) ;
#332 = DIRECTION ( 'NONE',  ( 1.550910762415513985E-16, 1.000000000000000000, -8.135128085091684243E-31 ) ) ;
#333 = EDGE_CURVE ( 'NONE', #15092, #15826, #3886, .T. ) ;
#334 = PLANE ( 'NONE',  #18718 ) ;
#335 = CARTESIAN_POINT ( 'NONE',  ( 0.3126073911696447549, 2.020725942163688504, 3.499999999999997780 ) ) ;
#336 = EDGE_CURVE ( 'NONE', #17272, #9446, #19746, .T. ) ;
#337 = ADVANCED_FACE ( 'NONE', ( #3665 ), #4392, .F. ) ;
#338 = STYLED_ITEM ( 'NONE', ( #9590 ), #11971 ) ;
#339 = EDGE_LOOP ( 'NONE', ( #16381, #10747, #21363, #15914, #5920, #9620 ) ) ;
#340 = CARTESIAN_POINT ( 'NONE',  ( -4.614318463248865854, 37.16513102274245028, -28.94121189041531750 ) ) ;
#341 = CIRCLE ( 'NONE', #13120, 4.750000000000000000 ) ;
#342 = DIRECTION ( 'NONE',  ( -1.000000000000000000, -3.254448077276381206E-32, -1.066788928082016908E-26 ) ) ;
#343 = VERTEX_POINT ( 'NONE', #19786 ) ;
#344 = AXIS2_PLACEMENT_3D ( 'NONE', #676, #7844, #18658 ) ;
#345 = VECTOR ( 'NONE', #22191, 1000.000000000000114 ) ;
#346 = CARTESIAN_POINT ( 'NONE',  ( 1.040834085586084257E-14, 4.500000000000003553, -1.499999999999994449 ) ) ;
#347 = CARTESIAN_POINT ( 'NONE',  ( 7.500000000000007105, -5.999999999999981348, 12.24999999999998224 ) ) ;
#348 = EDGE_CURVE ( 'NONE', #1547, #16744, #12832, .T. ) ;
#349 = CARTESIAN_POINT ( 'NONE',  ( 66.26395429947835680, -6.500000000000005329, -6.500000000000081712 ) ) ;
#350 = FACE_OUTER_BOUND ( 'NONE', #12361, .T. ) ;
#351 = DIRECTION ( 'NONE',  ( -1.000000000000000000, -2.699383410053119644E-30, -3.330669073875432643E-16 ) ) ;
#352 = ADVANCED_FACE ( 'NONE', ( #14705 ), #16571, .T. ) ;
#353 = EDGE_CURVE ( 'NONE', #9717, #9721, #18241, .T. ) ;
#354 = FACE_OUTER_BOUND ( 'NONE', #13443, .T. ) ;
#355 = LINE ( 'NONE', #4202, #16056 ) ;
#356 = CARTESIAN_POINT ( 'NONE',  ( 26.45000000029184051, 16.99999999900385461, -19.00000000000000355 ) ) ;
#357 = STYLED_ITEM ( 'NONE', ( #13468 ), #10311 ) ;
#358 = CARTESIAN_POINT ( 'NONE',  ( 7.651206356577058720, -13.16616768173521912, 8.300907142094251512 ) ) ;
#359 = DIRECTION ( 'NONE',  ( 1.000000000000000000, 1.910522504832140594E-31, -5.551115123125818447E-17 ) ) ;
#360 = CARTESIAN_POINT ( 'NONE',  ( 4.180345304246198879, 2.049116244671355336, -3.591763845239319242 ) ) ;
#361 = B_SPLINE_CURVE_WITH_KNOTS ( 'NONE', 3,
 ( #6764, #4763, #1473, #6888, #3009, #3129, #13933, #11933 ),
 .UNSPECIFIED., .F., .F.,
 ( 4, 2, 2, 4 ),
 ( 0.000000000000000000, 0.002450665683189822298, 0.003675998524784733663, 0.004901331366379645463 ),
 .UNSPECIFIED. ) ;
#362 = FACE_OUTER_BOUND ( 'NONE', #15798, .T. ) ;
#363 = ADVANCED_FACE ( 'NONE', ( #4339 ), #722, .F. ) ;
#364 = CARTESIAN_POINT ( 'NONE',  ( 1.999999999999974021, 3.464101615137785029, 3.469446951953614189E-15 ) ) ;
#365 = VECTOR ( 'NONE', #7293, 1000.000000000000000 ) ;
#366 = ADVANCED_FACE ( 'NONE', ( #833 ), #7887, .F. ) ;
#367 = CARTESIAN_POINT ( 'NONE',  ( 4.158921614371309694, -4.076055977742306879, 0.05993604794450200363 ) ) ;
#368 = EDGE_CURVE ( 'NONE', #2382, #9560, #3409, .T. ) ;
#369 = PRODUCT_CONTEXT ( 'NONE', #23224, 'mechanical' ) ;
#370 = EDGE_CURVE ( 'NONE', #12160, #6309, #12209, .T. ) ;
#371 = VERTEX_POINT ( 'NONE', #2699 ) ;
#372 = MECHANICAL_DESIGN_GEOMETRIC_PRESENTATION_REPRESENTATION (  '', ( #4867 ), #22164 ) ;
#374 = EDGE_LOOP ( 'NONE', ( #13092, #17364, #11552, #11898 ) ) ;
#373 = ORIENTED_EDGE ( 'NONE', *, *, #22479, .F. ) ;
#375 = CARTESIAN_POINT ( 'NONE',  ( 108.2426266706972058, -6.527605602963671316, -6.500000000000019540 ) ) ;
#376 = CARTESIAN_POINT ( 'NONE',  ( -3.999999999708139686, 49.99999999900385461, -29.00000000000000355 ) ) ;
#377 = DIRECTION ( 'NONE',  ( 0.2405376366294273427, 0.000000000000000000, -0.9706398123736372785 ) ) ;
#378 = ORIENTED_EDGE ( 'NONE', *, *, #16785, .T. ) ;
#379 = DIRECTION ( 'NONE',  ( -0.000000000000000000, -0.000000000000000000, 1.000000000000000000 ) ) ;
#380 = LINE ( 'NONE', #5677, #10534 ) ;
#381 = DIRECTION ( 'NONE',  ( 0.8660254037844354880, -0.5000000000000055511, 0.000000000000000000 ) ) ;
#382 = CARTESIAN_POINT ( 'NONE',  ( -4.470458892752995794, 37.36863211987452615, -16.03483522404608408 ) ) ;
#383 = CYLINDRICAL_SURFACE ( 'NONE', #5439, 2.550000000000000711 ) ;
#384 = CARTESIAN_POINT ( 'NONE',  ( 2.966164998648776141, 1.454929939081825330, -4.362451518707862519 ) ) ;
#385 = CARTESIAN_POINT ( 'NONE',  ( 3.999999999999955147, -2.309401076758532678, -0.5000000000000004441 ) ) ;
#386 = AXIS2_PLACEMENT_3D ( 'NONE', #9346, #14745, #22046 ) ;
#387 = CARTESIAN_POINT ( 'NONE',  ( 1.387778780781445676E-14, 4.618802153517020059, -0.3572655899081733644 ) ) ;
#388 = LINE ( 'NONE', #20141, #9445 ) ;
#389 = FACE_OUTER_BOUND ( 'NONE', #20121, .T. ) ;
#390 = CARTESIAN_POINT ( 'NONE',  ( 0.000000000000000000, -3.031088913245480576, 1.749999999999994671 ) ) ;
#391 = CARTESIAN_POINT ( 'NONE',  ( -0.5000000000000559552, -1.999999999999988010, -8.000000000000062172 ) ) ;
#392 = CARTESIAN_POINT ( 'NONE',  ( 7.345446946324464932, -0.2181520686730648306, 7.860330092053914974 ) ) ;
#393 = EDGE_CURVE ( 'NONE', #22556, #13205, #17081, .T. ) ;
#394 = EDGE_LOOP ( 'NONE', ( #15847, #9130, #15878, #21668 ) ) ;
#396 = VERTEX_POINT ( 'NONE', #16803 ) ;
#395 = ORIENTED_EDGE ( 'NONE', *, *, #6942, .F. ) ;
#397 = ORIENTED_EDGE ( 'NONE', *, *, #3887, .T. ) ;
#398 = ORIENTED_EDGE ( 'NONE', *, *, #14716, .T. ) ;
#400 = EDGE_LOOP ( 'NONE', ( #7462, #10799, #18667, #12854 ) ) ;
#399 = ORIENTED_EDGE ( 'NONE', *, *, #12220, .F. ) ;
#401 = AXIS2_PLACEMENT_3D ( 'NONE', #4614, #22620, #18981 ) ;
#402 = ORIENTED_EDGE ( 'NONE', *, *, #7849, .T. ) ;
#403 = CYLINDRICAL_SURFACE ( 'NONE', #5007, 2.549999999999997158 ) ;
#404 =( BOUNDED_SURFACE ( )  B_SPLINE_SURFACE ( 3, 2, ( 
 ( #12933, #11388, #19885 ),
 ( #2337, #3867, #21995 ),
 ( #16676, #20341, #11045 ),
 ( #16449, #5881, #465 ),
 ( #1987, #21769, #358 ),
 ( #5654, #9411, #3752 ),
 ( #13050, #20237, #11166 ),
 ( #587, #6112, #14923 ),
 ( #7871, #22109, #18578 ),
 ( #6001, #16555, #7527 ),
 ( #2228, #15035, #10918 ),
 ( #9177, #16338, #241 ),
 ( #7412, #20827, #6346 ),
 ( #4690, #13397, #13518 ) ),
 .UNSPECIFIED., .F., .F., .F. ) 
 B_SPLINE_SURFACE_WITH_KNOTS ( ( 4, 2, 2, 2, 2, 2, 4 ),
 ( 3, 3 ),
 ( 0.000000000000000000, 0.0009385527998839217345, 0.001407829199825882602, 0.001877105599767843469, 0.002346381999709804336, 0.002815658399651765204, 0.003754211199535686938 ),
 ( 0.000000000000000000, 1.000000000000000000 ),
 .UNSPECIFIED. ) 
 GEOMETRIC_REPRESENTATION_ITEM ( )  RATIONAL_B_SPLINE_SURFACE ( (
 ( 1.000000000000000000, 0.7071067811865469066, 1.000000000000000000),
 ( 1.000000000000000000, 0.7217349950160889538, 1.000000000000000000),
 ( 1.000000000000000000, 0.7325631490734629825, 1.000000000000000000),
 ( 1.000000000000000000, 0.7426392126584471232, 1.000000000000000000),
 ( 1.000000000000000000, 0.7449451721693458595, 1.000000000000000000),
 ( 1.000000000000000000, 0.7474053618999159099, 1.000000000000000000),
 ( 1.000000000000000000, 0.7475947887410098192, 1.000000000000000000),
 ( 1.000000000000000000, 0.7461109904165789120, 1.000000000000000000),
 ( 1.000000000000000000, 0.7444113185333037785, 1.000000000000000000),
 ( 1.000000000000000000, 0.7395217850810181792, 1.000000000000000000),
 ( 1.000000000000000000, 0.7363545993504778675, 1.000000000000000000),
 ( 1.000000000000000000, 0.7253814056383908193, 1.000000000000000000),
 ( 1.000000000000000000, 0.7159765610437973660, 1.000000000000000000),
 ( 1.000000000000000000, 0.7071067811865494601, 1.000000000000000000) ) ) 
 REPRESENTATION_ITEM ( '' )  SURFACE ( )  );
#405 = VERTEX_POINT ( 'NONE', #22365 ) ;
#406 = ORIENTED_EDGE ( 'NONE', *, *, #6745, .T. ) ;
#407 = CARTESIAN_POINT ( 'NONE',  ( 1.199999999999992628, 0.6000000000000103029, 4.543283425070376857 ) ) ;
#408 = DIRECTION ( 'NONE',  ( -7.860214984770699307E-18, 1.409037165336591006E-16, 1.000000000000000000 ) ) ;
#409 = DIRECTION ( 'NONE',  ( -2.220446049250313081E-16, 1.000000000000000000, -7.025792437124636392E-31 ) ) ;
#410 = CARTESIAN_POINT ( 'NONE',  ( 2.742413778650726108, -1.325747111984059590, 4.749999999999997335 ) ) ;
#411 = CARTESIAN_POINT ( 'NONE',  ( 4.175813232069149450, -2.061359961916378492, -3.570380186727402538 ) ) ;
#412 = DIRECTION ( 'NONE',  ( -1.000000000000000000, 0.000000000000000000, 0.000000000000000000 ) ) ;
#413 = FACE_OUTER_BOUND ( 'NONE', #17566, .T. ) ;
#414 = DIRECTION ( 'NONE',  ( 1.000000000000000000, 0.000000000000000000, 0.000000000000000000 ) ) ;
#415 = DIRECTION ( 'NONE',  ( 1.000000000000000000, -1.276756478318923119E-15, 1.239088197126283964E-15 ) ) ;
#416 = DIRECTION ( 'NONE',  ( 1.000000000000000000, 6.640738306473676004E-15, 4.078150875473213127E-31 ) ) ;
#417 = ORIENTED_EDGE ( 'NONE', *, *, #17478, .T. ) ;
#418 = FILL_AREA_STYLE_COLOUR ( '', #5602 ) ;
#419 = CARTESIAN_POINT ( 'NONE',  ( 0.000000000000000000, 0.000000000000000000, -25.03750572909317285 ) ) ;
#421 = ORIENTED_EDGE ( 'NONE', *, *, #13406, .T. ) ;
#420 = ORIENTED_EDGE ( 'NONE', *, *, #15029, .F. ) ;
#422 = ORIENTED_EDGE ( 'NONE', *, *, #14825, .T. ) ;
#423 = EDGE_LOOP ( 'NONE', ( #4977, #10308, #16171, #6608 ) ) ;
#424 = ORIENTED_EDGE ( 'NONE', *, *, #2047, .F. ) ;
#425 = ORIENTED_EDGE ( 'NONE', *, *, #22642, .T. ) ;
#426 = EDGE_CURVE ( 'NONE', #22532, #14335, #5472, .T. ) ;
#427 = ORIENTED_EDGE ( 'NONE', *, *, #3964, .F. ) ;
#428 = PLANE ( 'NONE',  #6939 ) ;
#429 = VECTOR ( 'NONE', #14345, 1000.000000000000000 ) ;
#430 = VECTOR ( 'NONE', #5625, 1000.000000000000114 ) ;
#431 = CARTESIAN_POINT ( 'NONE',  ( -12.85000000000001386, -14.00000000000005329, 2.550000000000052669 ) ) ;
#432 = CARTESIAN_POINT ( 'NONE',  ( 4.175075985190096262, -4.120741555260265088, -6.938893903907228378E-15 ) ) ;
#433 = DIRECTION ( 'NONE',  ( -1.000000000000000000, -3.254448077276381206E-32, -1.066788928082016908E-26 ) ) ;
#434 = DIRECTION ( 'NONE',  ( -1.000000000000000000, -3.254448077276381206E-32, -1.066788928082016908E-26 ) ) ;
#435 = DIRECTION ( 'NONE',  ( -1.000000000000000000, 4.190823558986610327E-31, -1.733449886265890494E-32 ) ) ;
#436 = CARTESIAN_POINT ( 'NONE',  ( -91.14322581977729953, 0.5000000000000073275, 6.823838874241844543 ) ) ;
#437 = LINE ( 'NONE', #1953, #9814 ) ;
#438 = CARTESIAN_POINT ( 'NONE',  ( -2.886699270652919314, 4.864326267994432129, -7.500000000000002665 ) ) ;
#439 = DIRECTION ( 'NONE',  ( -1.000000000000000000, 9.325873406851321250E-15, 0.000000000000000000 ) ) ;
#440 = CARTESIAN_POINT ( 'NONE',  ( 12.49999999999995914, 1.250000000000015099, -14.25000000000000178 ) ) ;
#441 =( LENGTH_UNIT ( ) NAMED_UNIT ( * ) SI_UNIT ( .MILLI., .METRE. ) );
#442 = DIRECTION ( 'NONE',  ( -1.550910762415566494E-16, -1.000000000000000000, 8.135128085091684243E-31 ) ) ;
#444 = VECTOR ( 'NONE', #613, 1000.000000000000000 ) ;
#443 = CARTESIAN_POINT ( 'NONE',  ( 4.030859730899538640, -1.403482646610872742, -3.500000000000009770 ) ) ;
#445 = CIRCLE ( 'NONE', #13220, 1.500000000000000000 ) ;
#446 = ADVANCED_FACE ( 'NONE', ( #19058 ), #22478, .F. ) ;
#447 = ORIENTED_EDGE ( 'NONE', *, *, #16080, .F. ) ;
#448 = EDGE_CURVE ( 'NONE', #12541, #7709, #4224, .T. ) ;
#449 = LINE ( 'NONE', #2321, #365 ) ;
#450 = DIRECTION ( 'NONE',  ( 3.032184104443272185E-30, 1.000000000000000000, -7.395570986447005381E-32 ) ) ;
#451 = ORIENTED_EDGE ( 'NONE', *, *, #16114, .F. ) ;
#452 = CARTESIAN_POINT ( 'NONE',  ( 37.00000000000006395, 10.75000000000000000, -10.43301270189220276 ) ) ;
#453 = CARTESIAN_POINT ( 'NONE',  ( -12.84999999999999964, -0.5000000000000038858, 5.750000000000018652 ) ) ;
#454 = CARTESIAN_POINT ( 'NONE',  ( -43.10883117545721888, 4.565685424949256443, -7.500000000000034639 ) ) ;
#455 = FACE_OUTER_BOUND ( 'NONE', #14770, .T. ) ;
#456 = EDGE_CURVE ( 'NONE', #6638, #13441, #21115, .T. ) ;
#457 = DIRECTION ( 'NONE',  ( -3.885780586188016830E-16, -4.437342591868156373E-31, 1.000000000000000000 ) ) ;
#458 = AXIS2_PLACEMENT_3D ( 'NONE', #20608, #18832, #22132 ) ;
#459 = VECTOR ( 'NONE', #20546, 1000.000000000000000 ) ;
#460 = CARTESIAN_POINT ( 'NONE',  ( -89.70000000000065654, 3.200000000000057021, -2.000000000000001776 ) ) ;
#461 = EDGE_CURVE ( 'NONE', #6874, #3000, #20486, .T. ) ;
#462 = CARTESIAN_POINT ( 'NONE',  ( 7.216878364870271234, 4.999999999999979572, -2.499999999999973799 ) ) ;
#463 = AXIS2_PLACEMENT_3D ( 'NONE', #5270, #12430, #19613 ) ;
#464 = DIRECTION ( 'NONE',  ( 0.000000000000000000, 0.000000000000000000, 1.000000000000000000 ) ) ;
#465 = CARTESIAN_POINT ( 'NONE',  ( 7.613388670473287156, -13.11165441297993084, 8.423574099071744925 ) ) ;
#466 = DIRECTION ( 'NONE',  ( 5.551115123125797493E-17, -2.869019762633797485E-16, -1.000000000000000000 ) ) ;
#467 = CARTESIAN_POINT ( 'NONE',  ( 61.83096495907209089, -4.753799060524588782, 6.500000000000179412 ) ) ;
#468 = CARTESIAN_POINT ( 'NONE',  ( 108.2426266706970353, -6.527605602963587828, 6.500000000000199840 ) ) ;
#469 = PRESENTATION_STYLE_ASSIGNMENT (( #14587 ) ) ;
#470 = CONICAL_SURFACE ( 'NONE', #11727, 2.054999999999999716, 0.7853981633974502774 ) ;
#471 = CARTESIAN_POINT ( 'NONE',  ( 42.50000000000014921, 2.999999999999999112, -14.99999999999998579 ) ) ;
#472 = EDGE_CURVE ( 'NONE', #1433, #3000, #8099, .T. ) ;
#473 = ADVANCED_FACE ( 'NONE', ( #13534 ), #11758, .F. ) ;
#474 = EDGE_CURVE ( 'NONE', #5438, #4432, #6471, .T. ) ;
#475 = B_SPLINE_CURVE_WITH_KNOTS ( 'NONE', 3,
 ( #19236, #2894, #11596, #1255 ),
 .UNSPECIFIED., .F., .F.,
 ( 4, 4 ),
 ( 0.01659225151561716932, 0.02095135962594951370 ),
 .UNSPECIFIED. ) ;
#476 = CIRCLE ( 'NONE', #11356, 0.4999999999999998335 ) ;
#477 = VERTEX_POINT ( 'NONE', #15401 ) ;
#478 = AXIS2_PLACEMENT_3D ( 'NONE', #12426, #1725, #23034 ) ;
#479 = AXIS2_PLACEMENT_3D ( 'NONE', #21483, #5360, #14060 ) ;
#480 = CONICAL_SURFACE ( 'NONE', #22650, 4.750000000000013323, 0.6593100683328582123 ) ;
#482 = EDGE_LOOP ( 'NONE', ( #12383, #18200, #19111, #4814 ) ) ;
#481 = ORIENTED_EDGE ( 'NONE', *, *, #4021, .F. ) ;
#483 = B_SPLINE_CURVE_WITH_KNOTS ( 'NONE', 3,
 ( #1623, #3166, #6801, #10448 ),
 .UNSPECIFIED., .F., .F.,
 ( 4, 4 ),
 ( 2.380735702043574917E-07, 0.002775112046897004661 ),
 .UNSPECIFIED. ) ;
#484 = EDGE_CURVE ( 'NONE', #1099, #2832, #13652, .T. ) ;
#485 = PLANE ( 'NONE',  #3877 ) ;
#486 = CARTESIAN_POINT ( 'NONE',  ( 0.000000000000000000, 0.000000000000000000, 0.000000000000000000 ) ) ;
#487 = CYLINDRICAL_SURFACE ( 'NONE', #2237, 0.5000000000000029976 ) ;
#489 = ORIENTED_EDGE ( 'NONE', *, *, #12121, .F. ) ;
#488 = EDGE_CURVE ( 'NONE', #8317, #12509, #8824, .T. ) ;
#490 = PLANE ( 'NONE',  #19494 ) ;
#491 = PLANE ( 'NONE',  #4882 ) ;
#492 = ADVANCED_FACE ( 'NONE', ( #12334 ), #15856, .T. ) ;
#493 = CARTESIAN_POINT ( 'NONE',  ( 24.74999999999999645, 0.2500000000000418554, -17.00000000000001066 ) ) ;
#494 = CARTESIAN_POINT ( 'NONE',  ( 0.02904021785398210737, -0.5999999999999895417, 3.399959840769905206 ) ) ;
#495 = SURFACE_SIDE_STYLE ('',( #16812 ) ) ;
#496 = CIRCLE ( 'NONE', #23096, 2.999999999999999112 ) ;
#497 = DIRECTION ( 'NONE',  ( -0.7071067811865475727, -0.7071067811865475727, 0.000000000000000000 ) ) ;
#498 = CIRCLE ( 'NONE', #14398, 0.4999999999999994449 ) ;
#499 = DIRECTION ( 'NONE',  ( -1.000000000000000000, -0.000000000000000000, -0.000000000000000000 ) ) ;
#500 = COLOUR_RGB ( '', 0.66274510, 0.83137255, 0.94901961) ;
#501 = DIRECTION ( 'NONE',  ( 1.454462294001240516E-30, 1.000000000000000000, 0.000000000000000000 ) ) ;
#502 = CIRCLE ( 'NONE', #2759, 2.249999999999996003 ) ;
#503 = LINE ( 'NONE', #14843, #76 ) ;
#504 = CIRCLE ( 'NONE', #11000, 0.5000000000000033307 ) ;
#505 = CARTESIAN_POINT ( 'NONE',  ( 4.175813232069142344, -4.122719923832743660, 0.000000000000000000 ) ) ;
#506 = CARTESIAN_POINT ( 'NONE',  ( -42.54314575050799618, 4.799999999999998934, 8.000000000000035527 ) ) ;
#507 = CARTESIAN_POINT ( 'NONE',  ( 0.000000000000000000, 0.000000000000000000, 0.000000000000000000 ) ) ;
#508 = CARTESIAN_POINT ( 'NONE',  ( 7.000000000000009770, -0.9711575687493200215, 9.522727272727296466 ) ) ;
#509 = ORIENTED_EDGE ( 'NONE', *, *, #11857, .T. ) ;
#511 = ORIENTED_EDGE ( 'NONE', *, *, #15896, .T. ) ;
#510 = ORIENTED_EDGE ( 'NONE', *, *, #22197, .F. ) ;
#512 = ORIENTED_EDGE ( 'NONE', *, *, #15274, .F. ) ;
#513 = ORIENTED_EDGE ( 'NONE', *, *, #17633, .T. ) ;
#514 = AXIS2_PLACEMENT_3D ( 'NONE', #18460, #4209, #9413 ) ;
#516 = EDGE_LOOP ( 'NONE', ( #5719, #17219, #15403, #12098, #8144, #13153, #18199, #8414 ) ) ;
#515 = ORIENTED_EDGE ( 'NONE', *, *, #15969, .F. ) ;
#517 = AXIS2_PLACEMENT_3D ( 'NONE', #18682, #14064, #6345 ) ;
#518 = ORIENTED_EDGE ( 'NONE', *, *, #5953, .T. ) ;
#519 = EDGE_CURVE ( 'NONE', #5606, #14358, #3300, .T. ) ;
#520 = CARTESIAN_POINT ( 'NONE',  ( -1.228174534879794922E-15, 2.686816014504568528, 2.346298152288371686 ) ) ;
#521 = AXIS2_PLACEMENT_3D ( 'NONE', #8817, #5413, #15970 ) ;
#522 = VERTEX_POINT ( 'NONE', #22826 ) ;
#523 = CIRCLE ( 'NONE', #891, 4.000000000000000000 ) ;
#524 = EDGE_LOOP ( 'NONE', ( #13786, #13583, #662, #2799 ) ) ;
#525 = AXIS2_PLACEMENT_3D ( 'NONE', #3093, #22741, #3329 ) ;
#526 = DIRECTION ( 'NONE',  ( -1.000000000000000000, -6.224605580259554159E-31, 2.887593071917436153E-31 ) ) ;
#527 = CARTESIAN_POINT ( 'NONE',  ( 0.1381419387119304232, -1.355287006778805647, -3.500000000000008882 ) ) ;
#528 = CARTESIAN_POINT ( 'NONE',  ( 4.197393957002244491, 7.205051708611501750E-14, -3.503767560748914711 ) ) ;
#529 = FACE_OUTER_BOUND ( 'NONE', #12268, .T. ) ;
#530 = ADVANCED_FACE ( 'NONE', ( #14233 ), #19524, .T. ) ;
#531 = LINE ( 'NONE', #7924, #22271 ) ;
#532 = DIRECTION ( 'NONE',  ( -1.000000000000000000, 2.312964634635739999E-16, -1.302601544865244959E-30 ) ) ;
#533 = CARTESIAN_POINT ( 'NONE',  ( 1.849731447979668930, 1.560358803171613351, -4.750000000000025757 ) ) ;
#534 = DIRECTION ( 'NONE',  ( 1.000000000000000000, -4.190823558986610327E-31, 1.733449886265890494E-32 ) ) ;
#535 = CARTESIAN_POINT ( 'NONE',  ( -89.70000000000054285, -9.020562075079396891E-14, 1.000000000000000888 ) ) ;
#536 = LINE ( 'NONE', #21829, #14939 ) ;
#537 = CONICAL_SURFACE ( 'NONE', #13676, 2.500000000000015543, 0.9599310885968873608 ) ;
#538 = VECTOR ( 'NONE', #11676, 1000.000000000000000 ) ;
#539 = CARTESIAN_POINT ( 'NONE',  ( 37.46001462128848658, 10.83019807384524391, -2.539985378711986819 ) ) ;
#540 = ORIENTED_EDGE ( 'NONE', *, *, #22390, .T. ) ;
#541 = FILL_AREA_STYLE ('',( #418 ) ) ;
#542 = DIRECTION ( 'NONE',  ( -4.003208021484906984E-16, 0.000000000000000000, 1.000000000000000000 ) ) ;
#544 = EDGE_LOOP ( 'NONE', ( #3998, #20221, #14255, #14599 ) ) ;
#543 = EDGE_LOOP ( 'NONE', ( #12301, #5370, #12717, #13469, #20277, #9943 ) ) ;
#545 =( REPRESENTATION_RELATIONSHIP ('NONE','NONE', #19450, #16280 ) REPRESENTATION_RELATIONSHIP_WITH_TRANSFORMATION ( #20350 )SHAPE_REPRESENTATION_RELATIONSHIP( ) );
#546 = EDGE_LOOP ( 'NONE', ( #13785, #3691, #515, #3410 ) ) ;
#547 = VERTEX_POINT ( 'NONE', #23069 ) ;
#548 = ORIENTED_EDGE ( 'NONE', *, *, #14303, .F. ) ;
#549 = ADVANCED_FACE ( 'NONE', ( #5291 ), #15517, .T. ) ;
#550 = DIRECTION ( 'NONE',  ( -1.000000000000000000, 7.477632011778292156E-48, -3.885780586188017323E-16 ) ) ;
#551 = AXIS2_PLACEMENT_3D ( 'NONE', #11797, #15781, #13457 ) ;
#552 = CLOSED_SHELL ( 'NONE', ( #5998, #12224, #22308, #16919, #14838, #610, #17542, #5814, #9022, #13526, #11262, #22008, #12800, #12847, #7373, #1350, #6364, #15263, #7801, #12373, #8928, #19017, #2140, #3076, #20370, #13608, #253, #7841, #18717, #10097, #22749, #10522, #2281, #5956, #13001, #8303, #15121, #2768, #13653, #19566, #15676, #20490, #22930, #18573, #22774, #6659, #16164, #8294, #8684, #5013, #2022, #6644, #17118, #6392, #7909, #19774, #10655, #21216, #20630, #3506, #12830, #8059, #21456, #15577, #6060, #7869, #10599, #15845, #17708, #12378, #6678, #19804, #5540, #19247, #5780, #21642, #16295, #19370, #13968, #12259, #9663, #1243, #17730, #12097, #1896, #687, #20297, #21117, #20746, #4689, #12071, #17436, #7470, #15967, #6389, #3205, #13846, #14982, #16297, #15524, #6855, #17451, #21619, #3605, #12668, #248, #4912, #22621, #14523, #15294, #7422, #169, #14422, #14548 ) ) ;
#553 = AXIS2_PLACEMENT_3D ( 'NONE', #6003, #7641, #3986 ) ;
#554 = FACE_OUTER_BOUND ( 'NONE', #6636, .T. ) ;
#555 = VERTEX_POINT ( 'NONE', #22710 ) ;
#556 = CIRCLE ( 'NONE', #18561, 5.200000000000001066 ) ;
#557 = EDGE_CURVE ( 'NONE', #19870, #14824, #11076, .T. ) ;
#558 = FACE_OUTER_BOUND ( 'NONE', #8377, .T. ) ;
#559 = CARTESIAN_POINT ( 'NONE',  ( -42.54314575050781144, -3.999999999999996447, -16.42537846091818210 ) ) ;
#560 = DIRECTION ( 'NONE',  ( 1.000000000000000000, 4.440892098500626162E-16, -5.551115123125782702E-16 ) ) ;
#561 = CARTESIAN_POINT ( 'NONE',  ( -6.958637496983413051, 36.00028509578874747, -18.50353548315064600 ) ) ;
#562 = CARTESIAN_POINT ( 'NONE',  ( -8.422565759993579704, -12.00000000000004441, 6.396710472006764903 ) ) ;
#563 = CARTESIAN_POINT ( 'NONE',  ( -7.604097569491910846, -13.58924811263090504, 8.440516644273101221 ) ) ;
#564 = CARTESIAN_POINT ( 'NONE',  ( 5.484827557301438894, 1.325747111984056037, 0.000000000000000000 ) ) ;
#565 = CARTESIAN_POINT ( 'NONE',  ( -50.65685424949274562, -3.200000000000091660, 8.000000000000062172 ) ) ;
#566 = CARTESIAN_POINT ( 'NONE',  ( -5.484827557301438894, 1.325747111984031834, 0.000000000000000000 ) ) ;
#567 = EDGE_CURVE ( 'NONE', #9447, #4397, #14113, .T. ) ;
#568 = SHAPE_REPRESENTATION_RELATIONSHIP ( 'NONE' , 'NONE' ,  #15574, #22653 ) ;
#569 = DIRECTION ( 'NONE',  ( 0.000000000000000000, 0.000000000000000000, 1.000000000000000000 ) ) ;
#570 = CARTESIAN_POINT ( 'NONE',  ( 3.948111298835275562, -0.6968132764965153658, -3.500000000000165645 ) ) ;
#571 = ORIENTED_EDGE ( 'NONE', *, *, #22014, .F. ) ;
#572 = EDGE_LOOP ( 'NONE', ( #5727, #7824, #20773, #18885 ) ) ;
#573 = CARTESIAN_POINT ( 'NONE',  ( 115.1426525620552894, -6.246200939475421876, 6.000000000000158096 ) ) ;
#574 = CARTESIAN_POINT ( 'NONE',  ( 0.000000000000000000, 0.000000000000000000, 0.000000000000000000 ) ) ;
#575 = ORIENTED_EDGE ( 'NONE', *, *, #21892, .T. ) ;
#576 = CARTESIAN_POINT ( 'NONE',  ( -6.000000000000199840, 4.799999999999935874, 8.000000000000035527 ) ) ;
#577 = CARTESIAN_POINT ( 'NONE',  ( 0.000000000000000000, 0.000000000000000000, -4.000000000000000000 ) ) ;
#578 = DIRECTION ( 'NONE',  ( 0.7071067811865510144, 0.7071067811865441310, -9.779905552809737959E-15 ) ) ;
#579 = CARTESIAN_POINT ( 'NONE',  ( -8.954763739086851970, -12.50000000000002132, 6.678571428571506097 ) ) ;
#580 = CIRCLE ( 'NONE', #8078, 2.500000000000000000 ) ;
#581 = CARTESIAN_POINT ( 'NONE',  ( -3.097832296507313600E-14, 60.00000000000000000, -4.249999999999968914 ) ) ;
#582 = CARTESIAN_POINT ( 'NONE',  ( -4.000000000000058620, -2.309401076758546445, -3.504269196027543387 ) ) ;
#583 = ORIENTED_EDGE ( 'NONE', *, *, #2070, .T. ) ;
#584 = CARTESIAN_POINT ( 'NONE',  ( 3.806148720138569086, 0.7500000000000555112, -3.000000000000023093 ) ) ;
#585 = CARTESIAN_POINT ( 'NONE',  ( 58.85734743794737511, 0.7537990605245015185, -6.499999999999895195 ) ) ;
#586 = EDGE_CURVE ( 'NONE', #15196, #6243, #21185, .T. ) ;
#587 = CARTESIAN_POINT ( 'NONE',  ( 7.490313984279763027, -13.85571552873294365, 7.566633644154762806 ) ) ;
#588 = LINE ( 'NONE', #7872, #10422 ) ;
#589 = DIRECTION ( 'NONE',  ( 0.6819983600624954789, 0.7313537016191733464, 7.771699578536739269E-16 ) ) ;
#590 = CARTESIAN_POINT ( 'NONE',  ( 66.26395429947839943, -7.000000000000006217, -6.499999999999999112 ) ) ;
#591 = EDGE_CURVE ( 'NONE', #7197, #2718, #10576, .T. ) ;
#592 = CARTESIAN_POINT ( 'NONE',  ( 4.086376042167607636, -4.082715877136866567, 0.07147133206917638537 ) ) ;
#593 = VECTOR ( 'NONE', #7277, 1000.000000000000000 ) ;
#594 = EDGE_CURVE ( 'NONE', #12892, #3237, #956, .T. ) ;
#595 = ITEM_DEFINED_TRANSFORMATION ( 'NONE', 'NONE', #13516,  #22115 ) ;
#596 = ORIENTED_EDGE ( 'NONE', *, *, #22450, .T. ) ;
#597 = EDGE_CURVE ( 'NONE', #11755, #7710, #15633, .T. ) ;
#599 = EDGE_LOOP ( 'NONE', ( #7573, #20564, #19035, #15482 ) ) ;
#598 = ORIENTED_EDGE ( 'NONE', *, *, #9835, .F. ) ;
#600 = CIRCLE ( 'NONE', #8864, 0.5000000000000028866 ) ;
#601 = DIRECTION ( 'NONE',  ( -1.000000000000000000, -2.699383410053119644E-30, -3.330669073875432643E-16 ) ) ;
#602 = CARTESIAN_POINT ( 'NONE',  ( 37.35148779274769026, 0.3618892054749011655, -2.648512207251555228 ) ) ;
#603 = AXIS2_PLACEMENT_3D ( 'NONE', #12913, #2082, #19970 ) ;
#604 = LINE ( 'NONE', #834, #21874 ) ;
#605 = ORIENTED_EDGE ( 'NONE', *, *, #6240, .F. ) ;
#606 = CARTESIAN_POINT ( 'NONE',  ( 12.49999999999997335, 1.500000000000015099, -9.500000000000001776 ) ) ;
#607 = DIRECTION ( 'NONE',  ( 0.7071067811865502373, -0.7071067811865447972, -5.485661035786110830E-15 ) ) ;
#608 = DIRECTION ( 'NONE',  ( 0.2405376366294550983, 0.000000000000000000, -0.9706398123736303951 ) ) ;
#610 = ADVANCED_FACE ( 'NONE', ( #4927 ), #12094, .F. ) ;
#609 = CARTESIAN_POINT ( 'NONE',  ( 0.8681510425101832684, -0.5999999999999895417, -4.444131413071498393 ) ) ;
#611 = EDGE_CURVE ( 'NONE', #9771, #21672, #8198, .T. ) ;
#612 = CARTESIAN_POINT ( 'NONE',  ( -1.660531772554314722, 3.660093687634845772, -5.600000000000003197 ) ) ;
#613 = DIRECTION ( 'NONE',  ( 1.000000000000000000, -4.437342591868175641E-31, 3.330669073875457788E-16 ) ) ;
#614 = DIRECTION ( 'NONE',  ( 0.000000000000000000, 0.000000000000000000, 1.000000000000000000 ) ) ;
#615 = DIRECTION ( 'NONE',  ( 1.000000000000000000, 0.000000000000000000, 0.000000000000000000 ) ) ;
#616 = FACE_BOUND ( 'NONE', #9219, .T. ) ;
#617 = EDGE_CURVE ( 'NONE', #18641, #4863, #6775, .T. ) ;
#619 = AXIS2_PLACEMENT_3D ( 'NONE', #4316, #2093, #7863 ) ;
#618 = FACE_OUTER_BOUND ( 'NONE', #20038, .T. ) ;
#620 = CARTESIAN_POINT ( 'NONE',  ( 4.071447262713884463, -2.020725942163709377, 3.500000000000003109 ) ) ;
#621 = FACE_OUTER_BOUND ( 'NONE', #4835, .T. ) ;
#622 = DIRECTION ( 'NONE',  ( -0.7071067811865475727, 0.7071067811865475727, 0.000000000000000000 ) ) ;
#623 = EDGE_CURVE ( 'NONE', #15916, #8376, #10912, .T. ) ;
#624 = ORIENTED_EDGE ( 'NONE', *, *, #1356, .F. ) ;
#625 = CIRCLE ( 'NONE', #16019, 2.500000000000000444 ) ;
#626 = EDGE_CURVE ( 'NONE', #2822, #21618, #7403, .T. ) ;
#628 = ORIENTED_EDGE ( 'NONE', *, *, #21380, .F. ) ;
#627 = ORIENTED_EDGE ( 'NONE', *, *, #1615, .F. ) ;
#629 = UNCERTAINTY_MEASURE_WITH_UNIT (LENGTH_MEASURE( 1.000000000000000082E-05 ), #16359, 'distance_accuracy_value', 'NONE');
#630 = ORIENTED_EDGE ( 'NONE', *, *, #14353, .F. ) ;
#632 = ORIENTED_EDGE ( 'NONE', *, *, #18856, .T. ) ;
#631 = ORIENTED_EDGE ( 'NONE', *, *, #9821, .T. ) ;
#633 = ORIENTED_EDGE ( 'NONE', *, *, #21096, .F. ) ;
#634 = DIRECTION ( 'NONE',  ( -1.000000000000000000, 4.440892098500650814E-16, 7.860214984771115307E-18 ) ) ;
#635 = VERTEX_POINT ( 'NONE', #18338 ) ;
#636 = EDGE_LOOP ( 'NONE', ( #3298, #20514, #22207, #18614 ) ) ;
#637 = DIRECTION ( 'NONE',  ( 3.330669073875457788E-16, 0.000000000000000000, -1.000000000000000000 ) ) ;
#638 = CIRCLE ( 'NONE', #21682, 2.550000000000002043 ) ;
#639 = CYLINDRICAL_SURFACE ( 'NONE', #14898, 2.549999999999997158 ) ;
#640 = DIRECTION ( 'NONE',  ( -0.000000000000000000, 1.000000000000000000, 4.190823558986611203E-31 ) ) ;
#641 = ADVANCED_FACE ( 'NONE', ( #120 ), #9980, .F. ) ;
#642 = CARTESIAN_POINT ( 'NONE',  ( 8.954763739086866181, -13.50000000000002309, 6.678571428571478563 ) ) ;
#643 = EDGE_CURVE ( 'NONE', #2718, #1098, #1705, .T. ) ;
#644 = FACE_OUTER_BOUND ( 'NONE', #16321, .T. ) ;
#645 = AXIS2_PLACEMENT_3D ( 'NONE', #22990, #1692, #8628 ) ;
#646 = ADVANCED_FACE ( 'NONE', ( #16203 ), #19002, .T. ) ;
#647 = CARTESIAN_POINT ( 'NONE',  ( 4.211405965630437898, 2.460463115436303028, -3.751298928144580547 ) ) ;
#648 = FACE_OUTER_BOUND ( 'NONE', #10629, .T. ) ;
#649 = CARTESIAN_POINT ( 'NONE',  ( 2.775557561562891351E-14, 8.499999999999984013, -0.4999999999999865663 ) ) ;
#650 = DIRECTION ( 'NONE',  ( 0.000000000000000000, 0.000000000000000000, 1.000000000000000000 ) ) ;
#651 = CARTESIAN_POINT ( 'NONE',  ( 0.000000000000000000, 0.000000000000000000, 0.000000000000000000 ) ) ;
#652 = B_SPLINE_CURVE_WITH_KNOTS ( 'NONE', 3,
 ( #20311, #7837, #2535, #432, #9723, #15003, #6073, #903, #7602, #16877, #7951, #15112, #4174, #21964, #22307, #6195 ),
 .UNSPECIFIED., .F., .F.,
 ( 4, 3, 3, 3, 3, 4 ),
 ( -2.111273352549518886E-06, 0.000000000000000000, 3.519286887793778349E-05, 7.191842652069384322E-05, 0.0001049868727093698859, 0.0001382836236822112402 ),
 .UNSPECIFIED. ) ;
#653 = EDGE_CURVE ( 'NONE', #19930, #15092, #3743, .T. ) ;
#654 = CARTESIAN_POINT ( 'NONE',  ( 0.2499999999999655276, 2.000000000000015543, -2.000000000000001776 ) ) ;
#655 = ORIENTED_EDGE ( 'NONE', *, *, #20733, .T. ) ;
#656 =( NAMED_UNIT ( * ) SI_UNIT ( $, .STERADIAN. ) SOLID_ANGLE_UNIT ( ) );
#658 = ORIENTED_EDGE ( 'NONE', *, *, #15288, .F. ) ;
#657 = EDGE_LOOP ( 'NONE', ( #7151, #5646, #14168, #8629 ) ) ;
#659 = AXIS2_PLACEMENT_3D ( 'NONE', #20444, #3967, #5749 ) ;
#660 = ORIENTED_EDGE ( 'NONE', *, *, #16140, .T. ) ;
#661 = AXIS2_PLACEMENT_3D ( 'NONE', #4718, #969, #19185 ) ;
#662 = ORIENTED_EDGE ( 'NONE', *, *, #21476, .T. ) ;
#663 = ORIENTED_EDGE ( 'NONE', *, *, #7766, .F. ) ;
#664 = CARTESIAN_POINT ( 'NONE',  ( 4.071447262713884463, -2.020725942163709377, 3.500000000000003109 ) ) ;
#665 = AXIS2_PLACEMENT_3D ( 'NONE', #19621, #7167, #5157 ) ;
#666 = CARTESIAN_POINT ( 'NONE',  ( 2.918498775983380256E-10, 2.999999999003851503, -12.99999999999999822 ) ) ;
#667 = ORIENTED_EDGE ( 'NONE', *, *, #10371, .T. ) ;
#668 = CYLINDRICAL_SURFACE ( 'NONE', #15478, 0.5000000000000004441 ) ;
#669 = DIRECTION ( 'NONE',  ( 1.000000000000000000, 2.699383410053119644E-30, 3.330669073875432643E-16 ) ) ;
#670 = DIRECTION ( 'NONE',  ( -1.000000000000000000, -1.479114197289397135E-31, -5.916456789157588541E-31 ) ) ;
#671 = VECTOR ( 'NONE', #10328, 1000.000000000000227 ) ;
#672 = DIRECTION ( 'NONE',  ( -9.693457064947022734E-26, 0.000000000000000000, 1.000000000000000000 ) ) ;
#673 = CARTESIAN_POINT ( 'NONE',  ( 4.175075985190096262, 4.120741555260244660, 0.000000000000000000 ) ) ;
#674 = AXIS2_PLACEMENT_3D ( 'NONE', #8315, #8440, #20912 ) ;
#675 = CARTESIAN_POINT ( 'NONE',  ( -4.000000000000095923, 0.9868501483902634153, -0.09357334158586104456 ) ) ;
#676 = CARTESIAN_POINT ( 'NONE',  ( 30.00000000029184832, -0.5000000009961480529, -5.999999999999998224 ) ) ;
#677 = DIRECTION ( 'NONE',  ( 3.032184104443272185E-30, 1.000000000000000000, -7.395570986447005381E-32 ) ) ;
#678 = AXIS2_PLACEMENT_3D ( 'NONE', #13630, #15379, #15731 ) ;
#679 = EDGE_CURVE ( 'NONE', #5232, #20512, #15973, .T. ) ;
#680 = FACE_OUTER_BOUND ( 'NONE', #17185, .T. ) ;
#681 = AXIS2_PLACEMENT_3D ( 'NONE', #3256, #17591, #7476 ) ;
#682 = AXIS2_PLACEMENT_3D ( 'NONE', #19335, #4745, #4857 ) ;
#683 = SURFACE_SIDE_STYLE ('',( #9387 ) ) ;
#684 = PLANE ( 'NONE',  #18357 ) ;
#685 = CARTESIAN_POINT ( 'NONE',  ( 0.1397371499201708889, 1.362866705336855722, 3.499999999999994227 ) ) ;
#686 = ORIENTED_EDGE ( 'NONE', *, *, #1852, .F. ) ;
#687 = ADVANCED_FACE ( 'NONE', ( #21534 ), #20120, .T. ) ;
#688 = VERTEX_POINT ( 'NONE', #10911 ) ;
#689 = ORIENTED_EDGE ( 'NONE', *, *, #18622, .F. ) ;
#690 = VERTEX_POINT ( 'NONE', #12574 ) ;
#691 = ORIENTED_EDGE ( 'NONE', *, *, #20005, .F. ) ;
#692 = AXIS2_PLACEMENT_3D ( 'NONE', #16136, #3905, #12614 ) ;
#693 = DIRECTION ( 'NONE',  ( 0.6819983600624958120, 0.7313537016191731244, 7.771699578536736311E-16 ) ) ;
#694 = LINE ( 'NONE', #5870, #6828 ) ;
#695 = EDGE_LOOP ( 'NONE', ( #13875, #14287, #3852, #8721 ) ) ;
#696 = FACE_OUTER_BOUND ( 'NONE', #6302, .T. ) ;
#697 = CARTESIAN_POINT ( 'NONE',  ( 2.250000000000001776, 2.697410439246579483E-14, 17.49999999999997513 ) ) ;
#698 = CARTESIAN_POINT ( 'NONE',  ( 2.775557561562891351E-14, 8.499999999999984013, -0.4999999999999865663 ) ) ;
#699 = AXIS2_PLACEMENT_3D ( 'NONE', #5072, #17177, #13549 ) ;
#700 = VERTEX_POINT ( 'NONE', #19396 ) ;
#701 = LINE ( 'NONE', #13282, #21174 ) ;
#702 = AXIS2_PLACEMENT_3D ( 'NONE', #5770, #9524, #20346 ) ;
#703 = CARTESIAN_POINT ( 'NONE',  ( 36.00000000029184832, 2.999999999003851503, -5.999999999999998224 ) ) ;
#704 = ORIENTED_EDGE ( 'NONE', *, *, #6611, .T. ) ;
#705 = CARTESIAN_POINT ( 'NONE',  ( 54.42435809754115894, 2.499999999999946709, 6.000000000000136779 ) ) ;
#706 = CARTESIAN_POINT ( 'NONE',  ( 8.160037397871480636, -13.99120688549555425, 6.662331851012024408 ) ) ;
#707 = CARTESIAN_POINT ( 'NONE',  ( 0.000000000000000000, -1.750000000000001554, 0.000000000000000000 ) ) ;
#708 = DIRECTION ( 'NONE',  ( 1.333893503340774882E-15, 2.778352770573747380E-17, 1.000000000000000000 ) ) ;
#709 = FACE_OUTER_BOUND ( 'NONE', #19574, .T. ) ;
#710 = CARTESIAN_POINT ( 'NONE',  ( 3.951447005078447372, 1.347150628109124115, -3.499999999999999112 ) ) ;
#711 = FILL_AREA_STYLE_COLOUR ( '', #14886 ) ;
#712 =( GEOMETRIC_REPRESENTATION_CONTEXT ( 3 ) GLOBAL_UNCERTAINTY_ASSIGNED_CONTEXT ( ( #16830 ) ) GLOBAL_UNIT_ASSIGNED_CONTEXT ( ( #5192, #21975, #2204 ) ) REPRESENTATION_CONTEXT ( 'NONE', 'WORKASPACE' ) );
#713 = CARTESIAN_POINT ( 'NONE',  ( -50.65685424949278826, 1.387778780781445676E-14, -7.500000000000034639 ) ) ;
#714 = EDGE_LOOP ( 'NONE', ( #13357, #3608, #9239, #4112 ) ) ;
#715 = CIRCLE ( 'NONE', #5215, 3.999999999999999112 ) ;
#716 = AXIS2_PLACEMENT_3D ( 'NONE', #8767, #5361, #3594 ) ;
#717 = ORIENTED_EDGE ( 'NONE', *, *, #22216, .T. ) ;
#719 = ORIENTED_EDGE ( 'NONE', *, *, #19907, .T. ) ;
#718 = ORIENTED_EDGE ( 'NONE', *, *, #16718, .F. ) ;
#720 = DIRECTION ( 'NONE',  ( 1.000000000000000000, 2.699383410053119644E-30, 3.330669073875432643E-16 ) ) ;
#721 = PRESENTATION_LAYER_ASSIGNMENT (  '', '', ( #18367 ) ) ;
#722 = PLANE ( 'NONE',  #20502 ) ;
#723 = ADVANCED_FACE ( 'NONE', ( #1644 ), #6821, .F. ) ;
#724 = PRESENTATION_STYLE_ASSIGNMENT (( #18824 ) ) ;
#725 = ORIENTED_EDGE ( 'NONE', *, *, #6094, .F. ) ;
#726 = CARTESIAN_POINT ( 'NONE',  ( 4.165266963751736995, 4.099263933823925399, 3.718842205176018431E-15 ) ) ;
#727 = LINE ( 'NONE', #18828, #3425 ) ;
#728 = DIRECTION ( 'NONE',  ( 1.000000000000000000, -4.615739097524200579E-16, -1.134196829589820086E-15 ) ) ;
#729 = CARTESIAN_POINT ( 'NONE',  ( -4.239424077913610311, 37.80035007138371839, -16.00730726111445534 ) ) ;
#730 = AXIS2_PLACEMENT_3D ( 'NONE', #8897, #17709, #6781 ) ;
#731 = DIRECTION ( 'NONE',  ( 0.000000000000000000, 0.000000000000000000, 1.000000000000000000 ) ) ;
#732 = CARTESIAN_POINT ( 'NONE',  ( 2.775557561562891351E-14, 2.999999999999992450, -0.4999999999999865663 ) ) ;
#733 = CARTESIAN_POINT ( 'NONE',  ( -6.938893903907228378E-14, 4.999999999999976907, -4.163336342344337027E-14 ) ) ;
#734 = DIRECTION ( 'NONE',  ( -2.168404344970994323E-16, 1.000000000000000000, -1.577721810442023611E-30 ) ) ;
#735 = CARTESIAN_POINT ( 'NONE',  ( 0.000000000000000000, 0.000000000000000000, 3.469446951953614189E-15 ) ) ;
#736 = VECTOR ( 'NONE', #1530, 1000.000000000000000 ) ;
#737 = CARTESIAN_POINT ( 'NONE',  ( -4.000000000000059508, -1.539600717839031629, -3.300726591567086032 ) ) ;
#738 = B_SPLINE_CURVE_WITH_KNOTS ( 'NONE', 3,
 ( #10637, #10409, #16039, #1817 ),
 .UNSPECIFIED., .F., .F.,
 ( 4, 4 ),
 ( 2.380737581550306806E-07, 0.002336974151641528670 ),
 .UNSPECIFIED. ) ;
#739 = CARTESIAN_POINT ( 'NONE',  ( 6.000000000291855429, -9.961476088449217059E-10, -39.00000000000000000 ) ) ;
#740 = EDGE_LOOP ( 'NONE', ( #2269, #18796, #14103, #12386 ) ) ;
#741 =( NAMED_UNIT ( * ) SI_UNIT ( $, .STERADIAN. ) SOLID_ANGLE_UNIT ( ) );
#743 = ORIENTED_EDGE ( 'NONE', *, *, #17717, .F. ) ;
#742 = ORIENTED_EDGE ( 'NONE', *, *, #2797, .T. ) ;
#744 = ORIENTED_EDGE ( 'NONE', *, *, #11852, .F. ) ;
#745 = EDGE_CURVE ( 'NONE', #15339, #15772, #17431, .T. ) ;
#746 = VERTEX_POINT ( 'NONE', #5056 ) ;
#748 = ORIENTED_EDGE ( 'NONE', *, *, #11622, .T. ) ;
#747 = ORIENTED_EDGE ( 'NONE', *, *, #64, .T. ) ;
#749 = VERTEX_POINT ( 'NONE', #21648 ) ;
#750 = LINE ( 'NONE', #7915, #20802 ) ;
#751 = CARTESIAN_POINT ( 'NONE',  ( -49.51923881554282048, 1.137615433949801247, 7.500000000000062172 ) ) ;
#752 = EDGE_CURVE ( 'NONE', #15489, #3212, #12450, .T. ) ;
#753 = ORIENTED_EDGE ( 'NONE', *, *, #1882, .T. ) ;
#754 = DIRECTION ( 'NONE',  ( 0.000000000000000000, 0.000000000000000000, 1.000000000000000000 ) ) ;
#755 = AXIS2_PLACEMENT_3D ( 'NONE', #13105, #409, #21706 ) ;
#756 = DIRECTION ( 'NONE',  ( -1.000000000000000000, -1.479114197289388027E-30, 2.013525853228518840E-32 ) ) ;
#757 = CARTESIAN_POINT ( 'NONE',  ( 1.200000000000006617, 0.6000000000000067502, -4.543283425070335113 ) ) ;
#758 = DIRECTION ( 'NONE',  ( 5.551115123125782702E-16, 1.201780285297635172E-31, -1.000000000000000000 ) ) ;
#759 = PRODUCT_DEFINITION_FORMATION_WITH_SPECIFIED_SOURCE ( 'ANY', '', #8169, .NOT_KNOWN. ) ;
#760 = CARTESIAN_POINT ( 'NONE',  ( -7.521298409251860662, -2.242072331701493670, 8.817899680514866390 ) ) ;
#761 = EDGE_CURVE ( 'NONE', #18638, #13378, #23145, .T. ) ;
#762 = DIRECTION ( 'NONE',  ( -0.000000000000000000, 1.000000000000000000, -0.000000000000000000 ) ) ;
#763 = LINE ( 'NONE', #20873, #11220 ) ;
#764 = EDGE_CURVE ( 'NONE', #8174, #11574, #3261, .T. ) ;
#765 = CARTESIAN_POINT ( 'NONE',  ( -12.84999999999999964, -2.000000000000001776, 0.000000000000000000 ) ) ;
#766 = EDGE_CURVE ( 'NONE', #11435, #5256, #21184, .T. ) ;
#767 = CARTESIAN_POINT ( 'NONE',  ( 0.000000000000000000, 0.000000000000000000, -5.000000000000000888 ) ) ;
#768 = CARTESIAN_POINT ( 'NONE',  ( -95.20000000000061391, -0.5000000000000975886, 8.000000000000117240 ) ) ;
#769 = CARTESIAN_POINT ( 'NONE',  ( 0.000000000000000000, 0.000000000000000000, -5.600000000000000533 ) ) ;
#770 = CARTESIAN_POINT ( 'NONE',  ( 2.918498775983380256E-10, -9.961476088449217059E-10, -45.00000000000000000 ) ) ;
#771 = EDGE_LOOP ( 'NONE', ( #10334, #9517, #6211, #11513, #11978, #14081 ) ) ;
#772 = SHAPE_REPRESENTATION_RELATIONSHIP ( 'NONE' , 'NONE' ,  #22944, #7243 ) ;
#773 = CIRCLE ( 'NONE', #10164, 0.5000000000000038858 ) ;
#775 = EDGE_LOOP ( 'NONE', ( #12033, #10591 ) ) ;
#774 = VERTEX_POINT ( 'NONE', #1977 ) ;
#776 = ADVANCED_FACE ( 'NONE', ( #15751 ), #4354, .T. ) ;
#777 = ORIENTED_EDGE ( 'NONE', *, *, #17393, .T. ) ;
#778 = EDGE_CURVE ( 'NONE', #20423, #3633, #5417, .T. ) ;
#779 = EDGE_CURVE ( 'NONE', #4281, #1775, #20143, .T. ) ;
#780 = ORIENTED_EDGE ( 'NONE', *, *, #14197, .F. ) ;
#781 = ORIENTED_EDGE ( 'NONE', *, *, #14027, .T. ) ;
#782 = ORIENTED_EDGE ( 'NONE', *, *, #10105, .F. ) ;
#783 = DIRECTION ( 'NONE',  ( -1.333893503340774882E-15, -2.778352770573747380E-17, -1.000000000000000000 ) ) ;
#784 = CARTESIAN_POINT ( 'NONE',  ( 5.599999999999994316, -4.041451884327383226, 0.000000000000000000 ) ) ;
#785 = ADVANCED_FACE ( 'NONE', ( #8823 ), #7065, .F. ) ;
#786 = ORIENTED_EDGE ( 'NONE', *, *, #13748, .F. ) ;
#787 = DIRECTION ( 'NONE',  ( 1.000000000000000000, 1.424116703980846297E-16, -1.095779650622964657E-32 ) ) ;
#788 = EDGE_CURVE ( 'NONE', #15578, #6044, #1862, .T. ) ;
#789 = DIRECTION ( 'NONE',  ( 0.000000000000000000, 0.000000000000000000, 1.000000000000000000 ) ) ;
#790 = CYLINDRICAL_SURFACE ( 'NONE', #17982, 2.550000000000003819 ) ;
#791 = AXIS2_PLACEMENT_3D ( 'NONE', #11762, #9654, #13189 ) ;
#792 = DIRECTION ( 'NONE',  ( 0.9706398123736330597, 1.110223024625160485E-16, 0.2405376366294442736 ) ) ;
#793 = CARTESIAN_POINT ( 'NONE',  ( -7.568091547083489523, -11.30436690654930310, 8.516664522246358615 ) ) ;
#794 = CARTESIAN_POINT ( 'NONE',  ( -7.856071383949657871, -13.95231939088843021, 7.015054140272262373 ) ) ;
#795 = CARTESIAN_POINT ( 'NONE',  ( 6.500000000000227374, 2.500000000000196287, 6.000000000000213163 ) ) ;
#796 = CARTESIAN_POINT ( 'NONE',  ( -6.938893903907228378E-14, -4.618802153517020059, -5.242734410091827613 ) ) ;
#797 = FILL_AREA_STYLE ('',( #2314 ) ) ;
#798 = DIRECTION ( 'NONE',  ( 1.000000000000000000, 1.479114197289387852E-30, -2.013525853228518840E-32 ) ) ;
#799 = CARTESIAN_POINT ( 'NONE',  ( -12.84999999999999964, -1.500000000000001332, 5.750000000000005329 ) ) ;
#800 = VERTEX_POINT ( 'NONE', #7297 ) ;
#801 = ORIENTED_EDGE ( 'NONE', *, *, #10616, .F. ) ;
#802 = AXIS2_PLACEMENT_3D ( 'NONE', #12809, #5296, #239 ) ;
#803 = AXIS2_PLACEMENT_3D ( 'NONE', #4880, #13195, #16816 ) ;
#804 = ORIENTED_EDGE ( 'NONE', *, *, #20468, .F. ) ;
#805 = ORIENTED_EDGE ( 'NONE', *, *, #9969, .T. ) ;
#806 = DIRECTION ( 'NONE',  ( -0.5000000000000038858, -0.8660254037844364872, -6.910079924703072041E-16 ) ) ;
#807 = CARTESIAN_POINT ( 'NONE',  ( -12.84999999999999964, -1.500000000000001332, 0.000000000000000000 ) ) ;
#808 = ORIENTED_EDGE ( 'NONE', *, *, #21708, .T. ) ;
#809 = B_SPLINE_CURVE_WITH_KNOTS ( 'NONE', 3,
 ( #13972, #21165, #12198, #1513, #14095, #21281, #3840, #18320, #5628, #11357, #21972, #19968, #19857, #9491, #4079, #7847 ),
 .UNSPECIFIED., .F., .F.,
 ( 4, 2, 2, 2, 2, 2, 2, 4 ),
 ( 2.168404344970985372E-18, 0.0008458391445145506393, 0.001268758716771827043, 0.001691678289029103664, 0.002114597861286380068, 0.002537517433543656688, 0.002960437005800932875, 0.003383356578058209496 ),
 .UNSPECIFIED. ) ;
#810 = DIRECTION ( 'NONE',  ( 1.000000000000000000, 3.081487911019581306E-31, -5.551115123125761132E-17 ) ) ;
#811 = EDGE_CURVE ( 'NONE', #17281, #16004, #992, .T. ) ;
#812 = FACE_OUTER_BOUND ( 'NONE', #7748, .T. ) ;
#813 = CARTESIAN_POINT ( 'NONE',  ( -45.91923881554279774, 2.462384566050190848, -7.500000000000062172 ) ) ;
#814 = CARTESIAN_POINT ( 'NONE',  ( -89.70000000000057128, -0.5000000000000628386, -2.000000000000001776 ) ) ;
#815 = CARTESIAN_POINT ( 'NONE',  ( -4.000000000000058620, -2.309401076758546445, -3.433295621305388678 ) ) ;
#816 = CARTESIAN_POINT ( 'NONE',  ( 6.500000000000366818, 2.500000000000196287, 6.500000000000123457 ) ) ;
#817 = EDGE_CURVE ( 'NONE', #5639, #8174, #15026, .T. ) ;
#818 = DIRECTION ( 'NONE',  ( -0.000000000000000000, 1.000000000000000000, -0.000000000000000000 ) ) ;
#819 = CARTESIAN_POINT ( 'NONE',  ( 2.918498775983380256E-10, 2.999999999003851503, -29.00000000000000355 ) ) ;
#820 = LINE ( 'NONE', #15157, #19828 ) ;
#821 = AXIS2_PLACEMENT_3D ( 'NONE', #3851, #21982, #16435 ) ;
#822 = CARTESIAN_POINT ( 'NONE',  ( -4.330127018922234505, 4.689110867544671102, -7.500000000000000000 ) ) ;
#823 = CARTESIAN_POINT ( 'NONE',  ( 2.499999999999971134, 4.250000000000003553, -1.500000000000029088 ) ) ;
#824 = DIRECTION ( 'NONE',  ( 0.8191520442889927978, 1.003171929053525979E-16, -0.5735764363510447161 ) ) ;
#825 = CARTESIAN_POINT ( 'NONE',  ( 4.175075985190096262, 2.060370777630125882, -3.568666869285561649 ) ) ;
#826 = ORIENTED_EDGE ( 'NONE', *, *, #17744, .F. ) ;
#827 = ORIENTED_EDGE ( 'NONE', *, *, #22142, .T. ) ;
#829 = EDGE_LOOP ( 'NONE', ( #9472, #14648, #21204, #1235, #22182, #6330 ) ) ;
#828 = ORIENTED_EDGE ( 'NONE', *, *, #7076, .T. ) ;
#830 = AXIS2_PLACEMENT_3D ( 'NONE', #9486, #8070, #792 ) ;
#831 = CIRCLE ( 'NONE', #9848, 4.000000000000045297 ) ;
#832 = DIRECTION ( 'NONE',  ( -1.000000000000000000, 0.000000000000000000, 0.000000000000000000 ) ) ;
#833 = FACE_OUTER_BOUND ( 'NONE', #12010, .T. ) ;
#834 = CARTESIAN_POINT ( 'NONE',  ( 4.000000000000003553, -2.309401076758539784, -5.600000000000000533 ) ) ;
#835 = ORIENTED_EDGE ( 'NONE', *, *, #15747, .T. ) ;
#836 = CARTESIAN_POINT ( 'NONE',  ( -95.70000000000062812, -1.318389841742373392E-13, 8.000000000000062172 ) ) ;
#837 = CARTESIAN_POINT ( 'NONE',  ( -45.37157287525414517, -6.828427124746218269, 7.500000000000089706 ) ) ;
#838 = PRODUCT ( 'Rod', 'Rod', '', ( #5665 ) ) ;
#839 = DIRECTION ( 'NONE',  ( 0.7071067811865474617, -0.7071067811865474617, 0.000000000000000000 ) ) ;
#840 = DIRECTION ( 'NONE',  ( 1.000000000000000000, -2.168404344971017743E-16, 1.203141491611691375E-30 ) ) ;
#841 = CARTESIAN_POINT ( 'NONE',  ( 0.000000000000000000, -1.750000000000001554, 0.000000000000000000 ) ) ;
#842 = AXIS2_PLACEMENT_3D ( 'NONE', #19098, #1117, #4968 ) ;
#843 = DIRECTION ( 'NONE',  ( 1.000000000000000000, 0.000000000000000000, 4.336808689941968432E-16 ) ) ;
#844 = CARTESIAN_POINT ( 'NONE',  ( -8.326672684688674053E-14, 4.999999999999893419, 7.499999999999958256 ) ) ;
#845 = DIRECTION ( 'NONE',  ( 0.000000000000000000, 1.000000000000000000, 0.000000000000000000 ) ) ;
#846 = FACE_OUTER_BOUND ( 'NONE', #19731, .T. ) ;
#847 = CARTESIAN_POINT ( 'NONE',  ( 0.000000000000000000, 3.031088913245508110, -1.750000000000029310 ) ) ;
#848 = DIRECTION ( 'NONE',  ( 2.168404344971008868E-16, 1.000000000000000000, 0.000000000000000000 ) ) ;
#849 = AXIS2_PLACEMENT_3D ( 'NONE', #4850, #17199, #11796 ) ;
#850 = CARTESIAN_POINT ( 'NONE',  ( 0.000000000000000000, 0.000000000000000000, -5.600000000000000533 ) ) ;
#852 = AXIS2_PLACEMENT_3D ( 'NONE', #14679, #3854, #11035 ) ;
#851 = CYLINDRICAL_SURFACE ( 'NONE', #5151, 0.5000000000000000000 ) ;
#853 = TOROIDAL_SURFACE ( 'NONE', #8348, 3.500000000000000888, 0.5000000000000000000 ) ;
#854 = EDGE_LOOP ( 'NONE', ( #1944, #11607, #22757, #20845 ) ) ;
#855 = ADVANCED_FACE ( 'NONE', ( #20227 ), #18262, .T. ) ;
#856 = AXIS2_PLACEMENT_3D ( 'NONE', #18442, #7510, #21754 ) ;
#857 = CARTESIAN_POINT ( 'NONE',  ( -86.51225780781811636, -25.34051643272968946, 56.66570243528393291 ) ) ;
#859 = EDGE_LOOP ( 'NONE', ( #22643, #18058, #20307, #6787 ) ) ;
#858 = ORIENTED_EDGE ( 'NONE', *, *, #16843, .T. ) ;
#860 = ORIENTED_EDGE ( 'NONE', *, *, #3116, .T. ) ;
#862 = ORIENTED_EDGE ( 'NONE', *, *, #5242, .F. ) ;
#861 = ORIENTED_EDGE ( 'NONE', *, *, #20330, .T. ) ;
#863 = TOROIDAL_SURFACE ( 'NONE', #8360, 4.366025403784441039, 0.5000000000000000000 ) ;
#864 = CARTESIAN_POINT ( 'NONE',  ( 3.999999999999948042, 2.309401076758532678, -3.433295621305378020 ) ) ;
#865 = LINE ( 'NONE', #22739, #9193 ) ;
#866 = EDGE_LOOP ( 'NONE', ( #15194, #20184, #2377, #21781 ) ) ;
#867 = AXIS2_PLACEMENT_3D ( 'NONE', #14945, #4006, #381 ) ;
#868 = CARTESIAN_POINT ( 'NONE',  ( 88.75737332930597745, -13.52760560296348302, 6.500000000000103029 ) ) ;
#869 = DIRECTION ( 'NONE',  ( -1.134196829589822059E-15, -6.741645191078037727E-32, 1.000000000000000000 ) ) ;
#870 = CIRCLE ( 'NONE', #1976, 0.5000000000000004441 ) ;
#871 = CARTESIAN_POINT ( 'NONE',  ( 37.43301270189236618, 10.75000000000000000, -2.999999999999988898 ) ) ;
#872 = AXIS2_PLACEMENT_3D ( 'NONE', #21088, #8383, #18976 ) ;
#873 = CARTESIAN_POINT ( 'NONE',  ( -50.65685424949273141, 0.000000000000000000, 8.000000000000076383 ) ) ;
#874 = CARTESIAN_POINT ( 'NONE',  ( 0.2500000000000036637, 2.000000000000001776, -17.00000000000000711 ) ) ;
#875 = FACE_OUTER_BOUND ( 'NONE', #22915, .T. ) ;
#876 =( NAMED_UNIT ( * ) PLANE_ANGLE_UNIT ( ) SI_UNIT ( $, .RADIAN. ) );
#877 = EDGE_CURVE ( 'NONE', #9710, #18942, #14680, .T. ) ;
#878 = CARTESIAN_POINT ( 'NONE',  ( -1.276902167985857367E-15, -2.859595677584336748, 2.047034997319572280 ) ) ;
#879 = LINE ( 'NONE', #16966, #14230 ) ;
#880 = CARTESIAN_POINT ( 'NONE',  ( -2.742413778650615086, 1.325747111984059590, -4.750000000000000888 ) ) ;
#881 = DIRECTION ( 'NONE',  ( -0.9878135252003118483, -1.627025617018325989E-30, 0.1556420233463091385 ) ) ;
#882 = VERTEX_POINT ( 'NONE', #18567 ) ;
#883 = EDGE_CURVE ( 'NONE', #16517, #14933, #8878, .T. ) ;
#884 = UNCERTAINTY_MEASURE_WITH_UNIT (LENGTH_MEASURE( 1.000000000000000082E-05 ), #16510, 'distance_accuracy_value', 'NONE');
#885 = AXIS2_PLACEMENT_3D ( 'NONE', #5509, #21519, #6803 ) ;
#886 =( NAMED_UNIT ( * ) PLANE_ANGLE_UNIT ( ) SI_UNIT ( $, .RADIAN. ) );
#888 = VERTEX_POINT ( 'NONE', #16668 ) ;
#887 = ORIENTED_EDGE ( 'NONE', *, *, #19737, .F. ) ;
#889 = VECTOR ( 'NONE', #18743, 1000.000000000000000 ) ;
#890 = AXIS2_PLACEMENT_3D ( 'NONE', #12840, #9317, #16129 ) ;
#891 = AXIS2_PLACEMENT_3D ( 'NONE', #18596, #17276, #8120 ) ;
#892 = ORIENTED_EDGE ( 'NONE', *, *, #22327, .T. ) ;
#893 = AXIS2_PLACEMENT_3D ( 'NONE', #20867, #8852, #2976 ) ;
#894 = ADVANCED_FACE ( 'NONE', ( #4093 ), #22410, .T. ) ;
#895 = ORIENTED_EDGE ( 'NONE', *, *, #16706, .T. ) ;
#896 = EDGE_CURVE ( 'NONE', #16369, #9334, #7402, .T. ) ;
#897 = ORIENTED_EDGE ( 'NONE', *, *, #10315, .T. ) ;
#898 = ADVANCED_FACE ( 'NONE', ( #12924 ), #16547, .T. ) ;
#899 = ORIENTED_EDGE ( 'NONE', *, *, #5134, .F. ) ;
#900 = CARTESIAN_POINT ( 'NONE',  ( 4.151274195509679465, -2.039912954708795745, 3.533232880573519363 ) ) ;
#901 = DIRECTION ( 'NONE',  ( 2.013525853228507892E-32, 6.902532920683810383E-31, -1.000000000000000000 ) ) ;
#902 = VERTEX_POINT ( 'NONE', #14802 ) ;
#903 = CARTESIAN_POINT ( 'NONE',  ( 4.151274195509675913, -4.079825909417513330, -2.794074523180553099E-14 ) ) ;
#904 = AXIS2_PLACEMENT_3D ( 'NONE', #1146, #20677, #16886 ) ;
#905 = DIRECTION ( 'NONE',  ( 4.190823558986625216E-31, -1.000000000000000000, 4.190823558986625216E-31 ) ) ;
#906 = VECTOR ( 'NONE', #1561, 1000.000000000000000 ) ;
#907 = DIRECTION ( 'NONE',  ( 9.470910429910634558E-17, 0.000000000000000000, -1.000000000000000000 ) ) ;
#908 = CARTESIAN_POINT ( 'NONE',  ( 2.499999999999992006, 4.250000000000003553, -3.469446951953614189E-14 ) ) ;
#909 = CIRCLE ( 'NONE', #17036, 0.5000000000000022204 ) ;
#910 = AXIS2_PLACEMENT_3D ( 'NONE', #13957, #10664, #16064 ) ;
#911 = CARTESIAN_POINT ( 'NONE',  ( -7.024848138041019041, -11.34038014973646646, 8.468562630484528952 ) ) ;
#912 = EDGE_CURVE ( 'NONE', #21589, #16716, #321, .T. ) ;
#913 = EDGE_CURVE ( 'NONE', #7934, #15346, #11036, .T. ) ;
#914 = CARTESIAN_POINT ( 'NONE',  ( -4.000000000000095923, 0.7924765000094626810, -0.05906175389896420325 ) ) ;
#915 = EDGE_CURVE ( 'NONE', #19164, #20509, #11154, .T. ) ;
#916 = CARTESIAN_POINT ( 'NONE',  ( 2.060000000000002718, 0.000000000000000000, -0.3080913168122707546 ) ) ;
#917 = FACE_OUTER_BOUND ( 'NONE', #16745, .T. ) ;
#918 = CARTESIAN_POINT ( 'NONE',  ( 37.57823792062865209, 0.08880391167987312928, -10.29045043747235333 ) ) ;
#919 = VERTEX_POINT ( 'NONE', #697 ) ;
#920 =( LENGTH_UNIT ( ) NAMED_UNIT ( * ) SI_UNIT ( .MILLI., .METRE. ) );
#921 = DIRECTION ( 'NONE',  ( -7.395570986446975166E-31, -3.382522293539642681E-32, -1.000000000000000000 ) ) ;
#922 = CARTESIAN_POINT ( 'NONE',  ( 7.000000000000006217, -5.999999999999981348, 6.250000000000005329 ) ) ;
#923 = ORIENTED_EDGE ( 'NONE', *, *, #303, .F. ) ;
#924 = EDGE_CURVE ( 'NONE', #20683, #3062, #16438, .T. ) ;
#925 = TOROIDAL_SURFACE ( 'NONE', #3908, 3.500000000000000000, 0.5000000000000000000 ) ;
#926 = EDGE_CURVE ( 'NONE', #3142, #12512, #18446, .T. ) ;
#927 = VERTEX_POINT ( 'NONE', #22218 ) ;
#928 = AXIS2_PLACEMENT_3D ( 'NONE', #22168, #18404, #9464 ) ;
#929 = ORIENTED_EDGE ( 'NONE', *, *, #11228, .T. ) ;
#930 = TOROIDAL_SURFACE ( 'NONE', #11052, 5.750000000000000000, 0.5000000000000000000 ) ;
#931 = ADVANCED_FACE ( 'NONE', ( #11380 ), #9509, .F. ) ;
#932 = FACE_OUTER_BOUND ( 'NONE', #10285, .T. ) ;
#933 = ORIENTED_EDGE ( 'NONE', *, *, #1286, .T. ) ;
#934 = DIRECTION ( 'NONE',  ( 0.000000000000000000, 0.000000000000000000, 1.000000000000000000 ) ) ;
#935 = DIRECTION ( 'NONE',  ( -0.7313537016191756779, 0.6819983600624930364, -4.478224685260177339E-16 ) ) ;
#936 = DIRECTION ( 'NONE',  ( 4.336808689942052446E-15, 1.000000000000000000, 3.574525976782710619E-31 ) ) ;
#937 = DIRECTION ( 'NONE',  ( 1.000000000000000000, -1.389842848855773367E-62, 2.013525853228507892E-32 ) ) ;
#938 = LINE ( 'NONE', #22804, #4058 ) ;
#939 = DIRECTION ( 'NONE',  ( -1.000000000000000000, 1.550910762415508562E-16, 0.000000000000000000 ) ) ;
#940 = DIRECTION ( 'NONE',  ( -9.121204216617949000E-31, -1.000000000000000000, 6.982962677686261977E-15 ) ) ;
#941 = DIRECTION ( 'NONE',  ( -1.000000000000000000, -2.699383410053119644E-30, -3.330669073875432643E-16 ) ) ;
#942 = CIRCLE ( 'NONE', #17063, 4.000000000000023093 ) ;
#943 = EDGE_CURVE ( 'NONE', #17067, #4165, #11494, .T. ) ;
#944 = DIRECTION ( 'NONE',  ( -1.000000000000000000, -0.000000000000000000, -0.000000000000000000 ) ) ;
#945 = DIRECTION ( 'NONE',  ( 3.254448077146059901E-32, 1.000000000000000000, 6.409494854920712161E-31 ) ) ;
#946 = CARTESIAN_POINT ( 'NONE',  ( -6.999999999708142795, 38.99999999900385461, -19.00000000000000355 ) ) ;
#947 = PLANE ( 'NONE',  #15243 ) ;
#948 = DIRECTION ( 'NONE',  ( -0.8571428571428582055, -3.574076823648845814E-15, -0.5150787536377109399 ) ) ;
#949 = ORIENTED_EDGE ( 'NONE', *, *, #8818, .F. ) ;
#950 = EDGE_CURVE ( 'NONE', #17683, #6944, #7745, .T. ) ;
#951 = CONTEXT_DEPENDENT_SHAPE_REPRESENTATION ( #4884, #8747 ) ;
#952 = ORIENTED_EDGE ( 'NONE', *, *, #22611, .T. ) ;
#953 = CIRCLE ( 'NONE', #7713, 7.499999999999998224 ) ;
#955 = VERTEX_POINT ( 'NONE', #16777 ) ;
#954 = EDGE_LOOP ( 'NONE', ( #18047, #18944, #13136, #596, #6750, #15540 ) ) ;
#956 = CIRCLE ( 'NONE', #20106, 3.933012701892234730 ) ;
#957 = FACE_OUTER_BOUND ( 'NONE', #16219, .T. ) ;
#958 = CARTESIAN_POINT ( 'NONE',  ( -12.85000000000001386, -14.00000000000007105, 5.551115123125782702E-14 ) ) ;
#959 = DIRECTION ( 'NONE',  ( 1.331202777560457422E-30, 1.000000000000000000, -7.395570986446985676E-31 ) ) ;
#960 = ORIENTED_EDGE ( 'NONE', *, *, #1744, .T. ) ;
#961 = DIRECTION ( 'NONE',  ( -1.000000000000000000, -2.699383410053119644E-30, -3.330669073875432643E-16 ) ) ;
#962 = DIRECTION ( 'NONE',  ( 1.333893503340774882E-15, 2.778352770573747380E-17, 1.000000000000000000 ) ) ;
#963 = CARTESIAN_POINT ( 'NONE',  ( 0.000000000000000000, 0.000000000000000000, 0.000000000000000000 ) ) ;
#964 = DIRECTION ( 'NONE',  ( -1.550910762415566494E-16, -1.000000000000000000, 8.135128085091684243E-31 ) ) ;
#965 = CARTESIAN_POINT ( 'NONE',  ( 1.999999999999974021, 3.464101615137785029, 3.469446951953614189E-15 ) ) ;
#966 = FACE_OUTER_BOUND ( 'NONE', #6498, .T. ) ;
#967 = CARTESIAN_POINT ( 'NONE',  ( 10.49999999999999467, -12.50000000000000711, 9.250000000000063949 ) ) ;
#968 = FACE_OUTER_BOUND ( 'NONE', #14289, .T. ) ;
#969 = DIRECTION ( 'NONE',  ( 1.000000000000000000, 3.254448077276381206E-32, 1.066788928082016908E-26 ) ) ;
#970 = COLOUR_RGB ( '', 0.40784314, 0.44705882, 0.49803922) ;
#971 = DIRECTION ( 'NONE',  ( 0.000000000000000000, 0.000000000000000000, 1.000000000000000000 ) ) ;
#972 = FACE_OUTER_BOUND ( 'NONE', #13994, .T. ) ;
#973 = DIRECTION ( 'NONE',  ( -1.000000000000000000, -2.699383410053119644E-30, -3.330669073875432643E-16 ) ) ;
#974 = EDGE_CURVE ( 'NONE', #18076, #3151, #3624, .T. ) ;
#975 = ORIENTED_EDGE ( 'NONE', *, *, #6535, .T. ) ;
#976 = AXIS2_PLACEMENT_3D ( 'NONE', #9197, #14370, #1677 ) ;
#978 = ORIENTED_EDGE ( 'NONE', *, *, #8806, .F. ) ;
#977 = ORIENTED_EDGE ( 'NONE', *, *, #23196, .F. ) ;
#979 = EDGE_CURVE ( 'NONE', #11432, #5256, #232, .T. ) ;
#980 = ORIENTED_EDGE ( 'NONE', *, *, #4067, .T. ) ;
#981 = SHAPE_REPRESENTATION ( 'hex flange nut gradea_iso_ISO - 4161 - M5 - N', ( #22115 ), #7475 ) ;
#983 = EDGE_LOOP ( 'NONE', ( #1133, #3126, #6569, #4982 ) ) ;
#982 = ORIENTED_EDGE ( 'NONE', *, *, #6089, .T. ) ;
#984 = CARTESIAN_POINT ( 'NONE',  ( -6.999999999708142795, 13.99999999900385106, -22.50000000000000000 ) ) ;
#985 = LINE ( 'NONE', #6982, #17847 ) ;
#986 = ORIENTED_EDGE ( 'NONE', *, *, #3342, .F. ) ;
#987 = FACE_OUTER_BOUND ( 'NONE', #17816, .T. ) ;
#988 = FACE_OUTER_BOUND ( 'NONE', #14105, .T. ) ;
#989 = DIRECTION ( 'NONE',  ( -0.000000000000000000, -0.000000000000000000, 1.000000000000000000 ) ) ;
#990 = CARTESIAN_POINT ( 'NONE',  ( -50.65685424949267457, -7.200000000000049916, 7.500000000000047962 ) ) ;
#991 = DIRECTION ( 'NONE',  ( -1.066786462891689527E-26, -6.656013887802287108E-31, -1.000000000000000000 ) ) ;
#992 = CIRCLE ( 'NONE', #11118, 0.2500000000000002220 ) ;
#993 = CARTESIAN_POINT ( 'NONE',  ( 30.00000000029184832, -9.961476088449217059E-10, -39.00000000000000000 ) ) ;
#994 = CARTESIAN_POINT ( 'NONE',  ( 5.100000000000000533, 6.368163355566246242E-16, -5.200000000000011724 ) ) ;
#995 = CARTESIAN_POINT ( 'NONE',  ( 4.033906725095055990, -1.419670120618832465, 3.499999999999995559 ) ) ;
#996 = FACE_OUTER_BOUND ( 'NONE', #14966, .T. ) ;
#997 = TOROIDAL_SURFACE ( 'NONE', #5495, 3.500000000000000888, 0.5000000000000000000 ) ;
#998 = DIRECTION ( 'NONE',  ( -1.000000000000000000, -4.440892098500626162E-16, 5.551115123125782702E-16 ) ) ;
#999 = CARTESIAN_POINT ( 'NONE',  ( 37.00000000000011369, 10.49999999999999822, -10.00000000000000888 ) ) ;
#1000 = DIRECTION ( 'NONE',  ( 3.885780586188016830E-16, 4.437342591868156373E-31, -1.000000000000000000 ) ) ;
#1001 = CARTESIAN_POINT ( 'NONE',  ( -6.000000000000074607, -8.000000000000003553, -7.500000000000034639 ) ) ;
#1002 = ORIENTED_EDGE ( 'NONE', *, *, #23103, .F. ) ;
#1003 = APPLICATION_PROTOCOL_DEFINITION ( 'draft international standard', 'automotive_design', 1998, #7881 ) ;
#1005 = ORIENTED_EDGE ( 'NONE', *, *, #896, .T. ) ;
#1004 = VERTEX_POINT ( 'NONE', #20924 ) ;
#1006 = ORIENTED_EDGE ( 'NONE', *, *, #15901, .F. ) ;
#1007 = VECTOR ( 'NONE', #1279, 1000.000000000000000 ) ;
#1008 = ORIENTED_EDGE ( 'NONE', *, *, #19202, .T. ) ;
#1009 = ORIENTED_EDGE ( 'NONE', *, *, #10614, .F. ) ;
#1010 = AXIS2_PLACEMENT_3D ( 'NONE', #8199, #4301, #10078 ) ;
#1011 = ORIENTED_EDGE ( 'NONE', *, *, #18784, .T. ) ;
#1012 = CARTESIAN_POINT ( 'NONE',  ( 4.071447262713884463, 2.020725942163688504, -3.499999999999999556 ) ) ;
#1013 = VECTOR ( 'NONE', #7217, 1000.000000000000000 ) ;
#1014 = CARTESIAN_POINT ( 'NONE',  ( -50.65685424949281668, 3.200000000000022382, 7.500000000000034639 ) ) ;
#1015 = ORIENTED_EDGE ( 'NONE', *, *, #15615, .T. ) ;
#1016 = DIRECTION ( 'NONE',  ( 1.000000000000000000, -1.858632295689435609E-16, 0.000000000000000000 ) ) ;
#1017 = DIRECTION ( 'NONE',  ( 1.000000000000000000, 0.000000000000000000, 0.000000000000000000 ) ) ;
#1018 = ADVANCED_FACE ( 'NONE', ( #13625 ), #18923, .F. ) ;
#1019 = FACE_OUTER_BOUND ( 'NONE', #2701, .T. ) ;
#1020 = CARTESIAN_POINT ( 'NONE',  ( -6.999999999708142795, 35.99999999900384751, -22.50000000000000000 ) ) ;
#1021 = DIRECTION ( 'NONE',  ( 2.220446049250313081E-16, -1.000000000000000000, 7.025792437124636392E-31 ) ) ;
#1022 = CARTESIAN_POINT ( 'NONE',  ( -7.854293383767468661, -11.68772904158800507, 7.820081954007019220 ) ) ;
#1023 = CARTESIAN_POINT ( 'NONE',  ( -8.204963667274178363, -13.91374178095054504, 7.312308861539002613 ) ) ;
#1024 = FACE_BOUND ( 'NONE', #9944, .T. ) ;
#1025 = EDGE_CURVE ( 'NONE', #18414, #9641, #4374, .T. ) ;
#1026 = VECTOR ( 'NONE', #15890, 1000.000000000000000 ) ;
#1027 = B_SPLINE_CURVE_WITH_KNOTS ( 'NONE', 3,
 ( #21795, #5679, #12838, #11417, #18604, #18254, #22246, #4347, #6134, #2477, #9315, #9656, #13313, #16811, #382, #729, #20493, #11527, #16358, #21901 ),
 .UNSPECIFIED., .F., .F.,
 ( 4, 2, 2, 2, 2, 2, 2, 2, 2, 4 ),
 ( 0.0005000078514897923158, 0.001232179299099195411, 0.001964350746708598289, 0.002696522194318001601, 0.003062607918122696102, 0.003428693641927389735, 0.004160865089536783072, 0.004893036537146174675, 0.005625207984755568012, 0.006357379432364960482 ),
 .UNSPECIFIED. ) ;
#1028 = CARTESIAN_POINT ( 'NONE',  ( 6.999999999999992006, -8.000000000000051514, 6.249999999999977796 ) ) ;
#1029 = DIRECTION ( 'NONE',  ( 0.000000000000000000, 0.000000000000000000, -1.000000000000000000 ) ) ;
#1030 = CIRCLE ( 'NONE', #4015, 0.5000000000000029976 ) ;
#1031 = EDGE_LOOP ( 'NONE', ( #7562, #11286, #14290 ) ) ;
#1032 = CIRCLE ( 'NONE', #19417, 4.000000000000023093 ) ;
#1033 = CARTESIAN_POINT ( 'NONE',  ( 4.033901012037268252, 2.321269032827638856, 2.979444097106773270 ) ) ;
#1034 = FACE_OUTER_BOUND ( 'NONE', #5261, .T. ) ;
#1035 = VERTEX_POINT ( 'NONE', #6220 ) ;
#1036 = AXIS2_PLACEMENT_3D ( 'NONE', #946, #10108, #20935 ) ;
#1037 = ORIENTED_EDGE ( 'NONE', *, *, #12723, .F. ) ;
#1038 = ORIENTED_EDGE ( 'NONE', *, *, #6940, .T. ) ;
#1039 = PRODUCT_DEFINITION_SHAPE ( 'NONE', 'NONE',  #23269 ) ;
#1040 = ORIENTED_EDGE ( 'NONE', *, *, #18309, .F. ) ;
#1041 = DIRECTION ( 'NONE',  ( 1.550910762415513985E-16, 1.000000000000000000, -8.135128085091684243E-31 ) ) ;
#1042 = EDGE_CURVE ( 'NONE', #11093, #19516, #20692, .T. ) ;
#1043 = DIRECTION ( 'NONE',  ( -4.190823558986626092E-31, 1.000000000000000000, 4.190823558986610327E-31 ) ) ;
#1044 = ORIENTED_EDGE ( 'NONE', *, *, #18492, .T. ) ;
#1045 = DIRECTION ( 'NONE',  ( 0.000000000000000000, -0.000000000000000000, 1.000000000000000000 ) ) ;
#1046 = FACE_OUTER_BOUND ( 'NONE', #14257, .T. ) ;
#1047 = B_SPLINE_CURVE_WITH_KNOTS ( 'NONE', 3,
 ( #15162, #21881, #12942, #825, #4215, #3990, #9762, #11397, #7876, #2578, #2110, #13057, #7994, #15038, #22231, #11171 ),
 .UNSPECIFIED., .F., .F.,
 ( 4, 3, 3, 3, 3, 4 ),
 ( -2.111273352577022893E-06, 0.000000000000000000, 3.519286887793240313E-05, 7.191842652067673993E-05, 0.0001049868727093628386, 0.0001382836236822181791 ),
 .UNSPECIFIED. ) ;
#1048 = AXIS2_PLACEMENT_3D ( 'NONE', #19388, #3733, #18095 ) ;
#1049 = CARTESIAN_POINT ( 'NONE',  ( 0.3126073911696378160, -2.020725942163709377, 3.500000000000003109 ) ) ;
#1050 = ADVANCED_FACE ( 'NONE', ( #4683 ), #7758, .T. ) ;
#1051 = DIRECTION ( 'NONE',  ( 1.550910762415566494E-16, 1.000000000000000000, -8.135128085091684243E-31 ) ) ;
#1052 = CARTESIAN_POINT ( 'NONE',  ( 4.030867648404781178, 3.732851566701672841, 0.5345114293579794618 ) ) ;
#1053 = AXIS2_PLACEMENT_3D ( 'NONE', #9891, #961, #12100 ) ;
#1054 = CARTESIAN_POINT ( 'NONE',  ( -92.25000000000065370, 5.494493748869900097E-14, -2.000000000000001776 ) ) ;
#1055 = DIRECTION ( 'NONE',  ( 9.693522803355793065E-26, -5.963788443470848352E-28, -1.000000000000000000 ) ) ;
#1056 = VECTOR ( 'NONE', #20372, 1000.000000000000000 ) ;
#1057 = CARTESIAN_POINT ( 'NONE',  ( -45.01801948466093961, 6.474873734152897242, -8.000000000000035527 ) ) ;
#1058 = EDGE_CURVE ( 'NONE', #11848, #1430, #638, .T. ) ;
#1059 = ADVANCED_FACE ( 'NONE', ( #812 ), #22427, .T. ) ;
#1060 = CARTESIAN_POINT ( 'NONE',  ( 119.5756419024615838, -6.500000000000061284, -5.999999999999984901 ) ) ;
#1061 = DIRECTION ( 'NONE',  ( -1.613696256722611405E-16, 0.000000000000000000, -1.000000000000000000 ) ) ;
#1063 = VECTOR ( 'NONE', #6055, 1000.000000000000000 ) ;
#1062 = CARTESIAN_POINT ( 'NONE',  ( -50.65685424949278826, 0.5000000000000213163, -7.500000000000034639 ) ) ;
#1064 = LINE ( 'NONE', #10212, #4061 ) ;
#1065 = AXIS2_PLACEMENT_3D ( 'NONE', #21849, #15010, #2543 ) ;
#1066 = AXIS2_PLACEMENT_3D ( 'NONE', #3230, #21463, #8745 ) ;
#1067 = ORIENTED_EDGE ( 'NONE', *, *, #6289, .F. ) ;
#1068 = ADVANCED_FACE ( 'NONE', ( #1046 ), #15491, .F. ) ;
#1069 = ADVANCED_FACE ( 'NONE', ( #22690 ), #22337, .T. ) ;
#1070 = AXIS2_PLACEMENT_3D ( 'NONE', #12709, #1992, #1876 ) ;
#1071 = EDGE_CURVE ( 'NONE', #22556, #2883, #22565, .T. ) ;
#1073 = ORIENTED_EDGE ( 'NONE', *, *, #6663, .T. ) ;
#1072 = VERTEX_POINT ( 'NONE', #4438 ) ;
#1074 = CIRCLE ( 'NONE', #6325, 5.500000000000000000 ) ;
#1075 = CARTESIAN_POINT ( 'NONE',  ( 59.19834661797866460, 1.119475911334100182, 6.500000000000130562 ) ) ;
#1076 = CARTESIAN_POINT ( 'NONE',  ( 37.00000000000011369, 11.00000000000000000, -6.499999999999950262 ) ) ;
#1077 = CARTESIAN_POINT ( 'NONE',  ( -6.549842551586334771, 36.00336057837468928, -26.38138186026117893 ) ) ;
#1078 = ORIENTED_EDGE ( 'NONE', *, *, #19074, .F. ) ;
#1079 = CARTESIAN_POINT ( 'NONE',  ( 2.499999999999998668, 2.000000000000001776, -17.75000000000000711 ) ) ;
#1080 = EDGE_CURVE ( 'NONE', #3914, #9423, #17915, .T. ) ;
#1081 = CARTESIAN_POINT ( 'NONE',  ( 7.499999999999978684, -8.000000000000051514, 6.249999999999977796 ) ) ;
#1082 = CARTESIAN_POINT ( 'NONE',  ( 35.50000000029184832, 2.999999999003851503, -19.00000000000000355 ) ) ;
#1083 = STYLED_ITEM ( 'NONE', ( #20322 ), #15045 ) ;
#1084 = CARTESIAN_POINT ( 'NONE',  ( -2.742413778650712342, 1.749999999999973799, 4.749999999999999112 ) ) ;
#1085 = PLANE ( 'NONE',  #6581 ) ;
#1086 = EDGE_CURVE ( 'NONE', #16898, #10112, #2677, .T. ) ;
#1087 = CARTESIAN_POINT ( 'NONE',  ( 35.50000000029184832, 2.999999999003851503, -18.50000000000000355 ) ) ;
#1088 = CARTESIAN_POINT ( 'NONE',  ( -50.65685424949274562, -2.700000000000125855, 7.500000000000076383 ) ) ;
#1089 = DIRECTION ( 'NONE',  ( 0.000000000000000000, 0.000000000000000000, 1.000000000000000000 ) ) ;
#1090 = AXIS2_PLACEMENT_3D ( 'NONE', #17003, #17354, #15598 ) ;
#1091 = AXIS2_PLACEMENT_3D ( 'NONE', #18092, #10900, #9266 ) ;
#1092 = DIRECTION ( 'NONE',  ( -1.000000000000000000, -1.479114197289388027E-30, 2.013525853228518840E-32 ) ) ;
#1093 = AXIS2_PLACEMENT_3D ( 'NONE', #20642, #18858, #1223 ) ;
#1094 = FACE_OUTER_BOUND ( 'NONE', #18101, .T. ) ;
#1095 = DIRECTION ( 'NONE',  ( -2.775557561562883647E-17, 3.406761633869147840E-16, -1.000000000000000000 ) ) ;
#1096 = ORIENTED_EDGE ( 'NONE', *, *, #3338, .T. ) ;
#1097 = CARTESIAN_POINT ( 'NONE',  ( -142.6487227650926286, 82.50018113422062527, 37.16570243528391870 ) ) ;
#1099 = VERTEX_POINT ( 'NONE', #13509 ) ;
#1098 = VERTEX_POINT ( 'NONE', #13743 ) ;
#1100 = PRESENTATION_LAYER_ASSIGNMENT (  '', '', ( #12342 ) ) ;
#1101 = EDGE_LOOP ( 'NONE', ( #16948, #7826, #13990, #15195 ) ) ;
#1103 = ORIENTED_EDGE ( 'NONE', *, *, #6153, .T. ) ;
#1102 = ORIENTED_EDGE ( 'NONE', *, *, #20925, .T. ) ;
#1104 = VERTEX_POINT ( 'NONE', #18803 ) ;
#1105 = CARTESIAN_POINT ( 'NONE',  ( -6.999999999999992006, -5.999999999999987566, 6.250000000000005329 ) ) ;
#1106 = CARTESIAN_POINT ( 'NONE',  ( 85.68838070902455684, -9.818697260249752645, 6.000000000000136779 ) ) ;
#1107 = AXIS2_PLACEMENT_3D ( 'NONE', #3565, #5092, #19911 ) ;
#1108 = CIRCLE ( 'NONE', #16476, 4.749999999999981348 ) ;
#1109 = DIRECTION ( 'NONE',  ( -0.4999999999999999445, -2.286725509617068974E-17, 0.8660254037844387076 ) ) ;
#1110 = EDGE_CURVE ( 'NONE', #11343, #15739, #11136, .T. ) ;
#1111 = DIRECTION ( 'NONE',  ( 3.032184104443272185E-30, 1.000000000000000000, -7.395570986447005381E-32 ) ) ;
#1112 = CARTESIAN_POINT ( 'NONE',  ( -8.719386969281453403, -1.499999991380633446, 6.820015264002448951 ) ) ;
#1113 = CARTESIAN_POINT ( 'NONE',  ( -12.85000000000005649, -13.50000000000011191, -6.249999999999921840 ) ) ;
#1114 = CARTESIAN_POINT ( 'NONE',  ( 4.203935335434104026, 1.640780671294174375, -3.598452447879221250 ) ) ;
#1115 = CARTESIAN_POINT ( 'NONE',  ( 10.49999999999996803, -0.5000000000000004441, 5.750000000000032863 ) ) ;
#1116 = DIRECTION ( 'NONE',  ( -0.7313537016191773432, 0.6819983600624913711, 1.628001950178159721E-16 ) ) ;
#1117 = DIRECTION ( 'NONE',  ( -1.000000000000000000, 4.190823558986610327E-31, -1.733449886265890494E-32 ) ) ;
#1118 = EDGE_CURVE ( 'NONE', #13735, #11435, #20927, .T. ) ;
#1119 = CARTESIAN_POINT ( 'NONE',  ( 0.2174200650117549538, -2.185595227304856447, 3.214438021527930456 ) ) ;
#1120 = CARTESIAN_POINT ( 'NONE',  ( 12.49999999999995914, 2.775557561562891351E-14, -9.500000000000003553 ) ) ;
#1121 = CARTESIAN_POINT ( 'NONE',  ( 1.199999999999992628, 0.6000000000000137446, 4.749999999999990230 ) ) ;
#1122 = DIRECTION ( 'NONE',  ( 3.885780586188016830E-16, 4.437342591868156373E-31, -1.000000000000000000 ) ) ;
#1123 = ADVANCED_FACE ( 'NONE', ( #22447 ), #17133, .T. ) ;
#1124 = ORIENTED_EDGE ( 'NONE', *, *, #13695, .F. ) ;
#1125 = PRODUCT_DEFINITION_CONTEXT ( 'detailed design', #2311, 'design' ) ;
#1127 = ORIENTED_EDGE ( 'NONE', *, *, #8585, .T. ) ;
#1126 = EDGE_LOOP ( 'NONE', ( #14306, #4368, #8291, #9544 ) ) ;
#1128 = ORIENTED_EDGE ( 'NONE', *, *, #17861, .F. ) ;
#1129 = EDGE_LOOP ( 'NONE', ( #13678, #18873, #19666 ) ) ;
#1130 = AXIS2_PLACEMENT_3D ( 'NONE', #16695, #21064, #22587 ) ;
#1131 = VERTEX_POINT ( 'NONE', #3036 ) ;
#1132 = PRODUCT_DEFINITION_FORMATION_WITH_SPECIFIED_SOURCE ( 'ANY', '', #838, .NOT_KNOWN. ) ;
#1133 = ORIENTED_EDGE ( 'NONE', *, *, #7575, .T. ) ;
#1134 = CARTESIAN_POINT ( 'NONE',  ( 4.104070371397483541, -2.023683613428362005, 3.505122836902511807 ) ) ;
#1135 = DIRECTION ( 'NONE',  ( 1.000000000000000000, 0.000000000000000000, 0.000000000000000000 ) ) ;
#1136 = VERTEX_POINT ( 'NONE', #10199 ) ;
#1137 = DIRECTION ( 'NONE',  ( 0.000000000000000000, -1.000000000000000000, 0.000000000000000000 ) ) ;
#1138 = DIRECTION ( 'NONE',  ( -3.885780586188016830E-16, -4.437342591868156373E-31, 1.000000000000000000 ) ) ;
#1139 = CARTESIAN_POINT ( 'NONE',  ( 0.000000000000000000, 1.750000000000001554, 0.000000000000000000 ) ) ;
#1140 = DIRECTION ( 'NONE',  ( 0.000000000000000000, 3.382522293539642133E-32, 1.000000000000000000 ) ) ;
#1141 = CARTESIAN_POINT ( 'NONE',  ( 4.630153689607049650, 0.000000000000000000, 0.000000000000000000 ) ) ;
#1142 = CARTESIAN_POINT ( 'NONE',  ( -6.962001439796708269, 35.99999999900384751, -26.47597002942762145 ) ) ;
#1143 = CARTESIAN_POINT ( 'NONE',  ( -7.756475484083226846, -13.93440482874970066, 7.145789564688727502 ) ) ;
#1144 = DIRECTION ( 'NONE',  ( -9.121204216617949000E-31, -1.000000000000000000, 6.982962677686276966E-15 ) ) ;
#1145 = AXIS2_PLACEMENT_3D ( 'NONE', #5595, #16499, #9229 ) ;
#1146 = CARTESIAN_POINT ( 'NONE',  ( 0.000000000000000000, 0.000000000000000000, 0.000000000000000000 ) ) ;
#1147 = PLANE ( 'NONE',  #16386 ) ;
#1148 = VERTEX_POINT ( 'NONE', #23035 ) ;
#1149 = SHAPE_REPRESENTATION_RELATIONSHIP ( 'NONE' , 'NONE' ,  #1164, #3571 ) ;
#1150 = CARTESIAN_POINT ( 'NONE',  ( 4.158921614371306141, 4.076055977742309544, -0.05993604794450450857 ) ) ;
#1151 = CARTESIAN_POINT ( 'NONE',  ( -55.05572809000119605, -0.5000000000001045830, -8.000000000000090594 ) ) ;
#1152 = ORIENTED_EDGE ( 'NONE', *, *, #12772, .F. ) ;
#1153 = EDGE_CURVE ( 'NONE', #19243, #10116, #19375, .T. ) ;
#1154 = ORIENTED_EDGE ( 'NONE', *, *, #9823, .F. ) ;
#1155 = VERTEX_POINT ( 'NONE', #1726 ) ;
#1156 = ORIENTED_EDGE ( 'NONE', *, *, #626, .F. ) ;
#1157 = ORIENTED_EDGE ( 'NONE', *, *, #788, .T. ) ;
#1158 = CARTESIAN_POINT ( 'NONE',  ( 0.000000000000000000, 0.000000000000000000, 0.000000000000000000 ) ) ;
#1159 = DIRECTION ( 'NONE',  ( -0.6819983600625064701, -0.7313537016191632434, 0.000000000000000000 ) ) ;
#1160 = ORIENTED_EDGE ( 'NONE', *, *, #10930, .T. ) ;
#1161 = AXIS2_PLACEMENT_3D ( 'NONE', #5449, #12957, #8972 ) ;
#1162 = DIRECTION ( 'NONE',  ( -1.066786462891689527E-26, -6.656013887802287108E-31, -1.000000000000000000 ) ) ;
#1163 = DIRECTION ( 'NONE',  ( 0.000000000000000000, 0.000000000000000000, 1.000000000000000000 ) ) ;
#1164 = SHAPE_REPRESENTATION ( 'Handle Clip', ( #22115 ), #13848 ) ;
#1165 = DIRECTION ( 'NONE',  ( 1.066786462891689527E-26, 6.656013887802287108E-31, 1.000000000000000000 ) ) ;
#1166 = CARTESIAN_POINT ( 'NONE',  ( 113.0166151911346617, -11.64708151429780258, 6.500000000000110134 ) ) ;
#1167 = DIRECTION ( 'NONE',  ( -1.000000000000000000, -4.440892098500626162E-16, 5.551115123125782702E-16 ) ) ;
#1168 = CARTESIAN_POINT ( 'NONE',  ( -7.742458795615052125, -0.7399311281351333980, 8.061568688625936119 ) ) ;
#1169 = CARTESIAN_POINT ( 'NONE',  ( 2.918498775983380256E-10, 6.999999999003851947, -26.00000000000000000 ) ) ;
#1170 = DIRECTION ( 'NONE',  ( 1.000000000000000000, 2.699383410053119644E-30, 3.330669073875432643E-16 ) ) ;
#1171 = LINE ( 'NONE', #18813, #22070 ) ;
#1172 = CARTESIAN_POINT ( 'NONE',  ( -42.54314575050796776, 3.999999999999996447, -8.000000000000035527 ) ) ;
#1173 = EDGE_CURVE ( 'NONE', #746, #20880, #10395, .T. ) ;
#1174 = CARTESIAN_POINT ( 'NONE',  ( -8.697224362267968800, -13.50000000000004263, 6.250000000000033751 ) ) ;
#1175 = AXIS2_PLACEMENT_3D ( 'NONE', #17283, #13886, #10583 ) ;
#1176 = EDGE_LOOP ( 'NONE', ( #59, #15142, #15367 ) ) ;
#1177 = ADVANCED_FACE ( 'NONE', ( #1503 ), #3393, .T. ) ;
#1178 = VERTEX_POINT ( 'NONE', #9026 ) ;
#1181 = ORIENTED_EDGE ( 'NONE', *, *, #21353, .T. ) ;
#1180 = ADVANCED_FACE ( 'NONE', ( #8796 ), #2504, .T. ) ;
#1179 = ORIENTED_EDGE ( 'NONE', *, *, #1875, .F. ) ;
#1182 = EDGE_CURVE ( 'NONE', #6492, #18669, #10552, .T. ) ;
#1183 = CARTESIAN_POINT ( 'NONE',  ( 24.74999999999996447, 1.500000000000043077, -2.000000000000005329 ) ) ;
#1184 = EDGE_CURVE ( 'NONE', #16673, #23235, #22737, .T. ) ;
#1185 = CARTESIAN_POINT ( 'NONE',  ( 2.775557561562891351E-14, 0.5000000000000004441, -3.000000000000002665 ) ) ;
#1186 = CARTESIAN_POINT ( 'NONE',  ( -2.742413778650615086, 1.325747111984059590, -4.750000000000000888 ) ) ;
#1187 = ORIENTED_EDGE ( 'NONE', *, *, #22325, .T. ) ;
#1188 = SPHERICAL_SURFACE ( 'NONE', #17017, 0.5000000000000000000 ) ;
#1189 = TOROIDAL_SURFACE ( 'NONE', #11309, 2.250000000000000444, 0.2500000000000000000 ) ;
#1190 = CIRCLE ( 'NONE', #19959, 7.200000000000046363 ) ;
#1191 = CARTESIAN_POINT ( 'NONE',  ( -55.05572809000130974, 2.700000000000021938, -8.000000000000035527 ) ) ;
#1192 = DIRECTION ( 'NONE',  ( -1.000000000000000000, -2.168404344971017743E-16, 1.780660105995169760E-30 ) ) ;
#1193 = CARTESIAN_POINT ( 'NONE',  ( 37.43301270189239460, 0.2500000000000002220, -9.999999999999953815 ) ) ;
#1194 = CARTESIAN_POINT ( 'NONE',  ( -42.54314575050792513, 3.999999999999996447, 16.42537846091821052 ) ) ;
#1195 = CARTESIAN_POINT ( 'NONE',  ( 1.387778780781445676E-14, 4.857225732735059864E-14, -1.500000000000001332 ) ) ;
#1196 = DIRECTION ( 'NONE',  ( -1.000000000000000000, 1.276756478318922725E-15, -1.333893503340766402E-15 ) ) ;
#1197 = CARTESIAN_POINT ( 'NONE',  ( -4.690415759823443942, 0.7500000000000770495, -2.000000000000001776 ) ) ;
#1198 = ADVANCED_FACE ( 'NONE', ( #1613 ), #13026, .T. ) ;
#1199 = EDGE_CURVE ( 'NONE', #1642, #6272, #16255, .T. ) ;
#1200 = CARTESIAN_POINT ( 'NONE',  ( 4.170895651974849905, -4.109780709045216973, 1.853155041415897988E-14 ) ) ;
#1201 = VERTEX_POINT ( 'NONE', #15951 ) ;
#1202 = SURFACE_STYLE_USAGE ( .BOTH. , #9911 ) ;
#1203 = AXIS2_PLACEMENT_3D ( 'NONE', #1141, #1478, #8650 ) ;
#1204 = AXIS2_PLACEMENT_3D ( 'NONE', #813, #11495, #13510 ) ;
#1206 = VERTEX_POINT ( 'NONE', #1388 ) ;
#1205 = ORIENTED_EDGE ( 'NONE', *, *, #8263, .F. ) ;
#1207 = ADVANCED_FACE ( 'NONE', ( #12547 ), #3613, .T. ) ;
#1208 = ORIENTED_EDGE ( 'NONE', *, *, #21026, .T. ) ;
#1211 = EDGE_LOOP ( 'NONE', ( #10687, #3, #21937, #717 ) ) ;
#1210 = EDGE_CURVE ( 'NONE', #23117, #22529, #21623, .T. ) ;
#1209 = EDGE_LOOP ( 'NONE', ( #6411, #6701, #20193 ) ) ;
#1212 = ORIENTED_EDGE ( 'NONE', *, *, #318, .T. ) ;
#1213 = CARTESIAN_POINT ( 'NONE',  ( -4.000000000000003553, 0.000000000000000000, 0.000000000000000000 ) ) ;
#1214 = ADVANCED_FACE ( 'NONE', ( #5498 ), #14910, .F. ) ;
#1215 = DIRECTION ( 'NONE',  ( 1.734723475976813750E-16, 1.000000000000000000, -3.469446951953607484E-15 ) ) ;
#1216 = DIRECTION ( 'NONE',  ( -1.000000000000000000, 6.938893903907186568E-15, 0.000000000000000000 ) ) ;
#1217 = AXIS2_PLACEMENT_3D ( 'NONE', #8285, #6518, #15441 ) ;
#1218 = CARTESIAN_POINT ( 'NONE',  ( 4.330127018922088844, -1.387778780781445676E-13, 7.500000000000027534 ) ) ;
#1219 = CARTESIAN_POINT ( 'NONE',  ( -7.028413389564923897, -0.6300521812368727881, 8.946655872545999699 ) ) ;
#1220 = CARTESIAN_POINT ( 'NONE',  ( -91.14322581977729953, 2.700000000000014833, 6.823838874241844543 ) ) ;
#1221 = CARTESIAN_POINT ( 'NONE',  ( 4.175813232069142344, -2.061359961916371830, -3.570380186727398986 ) ) ;
#1222 = CARTESIAN_POINT ( 'NONE',  ( -3.122502256758252770E-14, 59.74999999999991473, 2.081668171172168513E-14 ) ) ;
#1223 = DIRECTION ( 'NONE',  ( -1.000000000000000000, -1.144237745222090235E-17, 1.939787525279694125E-32 ) ) ;
#1224 = VECTOR ( 'NONE', #17612, 1000.000000000000114 ) ;
#1225 = DIRECTION ( 'NONE',  ( 0.1556420233463076119, 0.000000000000000000, 0.9878135252003121813 ) ) ;
#1226 = AXIS2_PLACEMENT_3D ( 'NONE', #7718, #9254, #20081 ) ;
#1227 = CARTESIAN_POINT ( 'NONE',  ( 4.630153689607049650, 0.000000000000000000, 0.000000000000000000 ) ) ;
#1228 = CIRCLE ( 'NONE', #14361, 0.5000000000000004441 ) ;
#1229 = DIRECTION ( 'NONE',  ( -0.000000000000000000, 1.000000000000000000, 4.190823558986611203E-31 ) ) ;
#1230 = CARTESIAN_POINT ( 'NONE',  ( -7.764145988665059228, -12.22513543353773002, 8.011880279048888553 ) ) ;
#1231 = FACE_OUTER_BOUND ( 'NONE', #3457, .T. ) ;
#1232 = CARTESIAN_POINT ( 'NONE',  ( 3.878096787214414753, -2.680238624820921345, 2.357690525401619830 ) ) ;
#1233 = PRODUCT_DEFINITION_SHAPE ( 'NONE', 'NONE',  #14519 ) ;
#1234 = ORIENTED_EDGE ( 'NONE', *, *, #8668, .F. ) ;
#1236 = ORIENTED_EDGE ( 'NONE', *, *, #23063, .T. ) ;
#1235 = ORIENTED_EDGE ( 'NONE', *, *, #20428, .F. ) ;
#1237 = EDGE_CURVE ( 'NONE', #4862, #16835, #16732, .T. ) ;
#1238 = ORIENTED_EDGE ( 'NONE', *, *, #15588, .F. ) ;
#1239 = ORIENTED_EDGE ( 'NONE', *, *, #2920, .T. ) ;
#1240 = AXIS2_PLACEMENT_3D ( 'NONE', #7811, #18512, #20522 ) ;
#1241 = AXIS2_PLACEMENT_3D ( 'NONE', #1247, #17337, #14055 ) ;
#1242 = CIRCLE ( 'NONE', #11361, 0.5000000000000029976 ) ;
#1243 = ADVANCED_FACE ( 'NONE', ( #18852 ), #10767, .T. ) ;
#1244 = CIRCLE ( 'NONE', #16614, 0.4999999999999997224 ) ;
#1245 = ORIENTED_EDGE ( 'NONE', *, *, #3629, .T. ) ;
#1246 = CARTESIAN_POINT ( 'NONE',  ( 5.599999999999994316, 0.000000000000000000, 0.000000000000000000 ) ) ;
#1247 = CARTESIAN_POINT ( 'NONE',  ( -42.54314575050785407, -4.000000000000034639, -7.500000000000007105 ) ) ;
#1248 = ORIENTED_EDGE ( 'NONE', *, *, #19903, .T. ) ;
#1249 = CARTESIAN_POINT ( 'NONE',  ( -50.65685424949263904, -7.200000000000071232, -7.500000000000034639 ) ) ;
#1250 = CARTESIAN_POINT ( 'NONE',  ( -1.110223024625156540E-13, -1.999999999999988010, 7.500000000000020428 ) ) ;
#1251 = CYLINDRICAL_SURFACE ( 'NONE', #10241, 2.500000000000000000 ) ;
#1252 = DIRECTION ( 'NONE',  ( -4.019602852144232182E-47, -6.982962677686261977E-15, -1.000000000000000000 ) ) ;
#1253 = DIRECTION ( 'NONE',  ( -0.7313537016191753448, -0.6819983600624934805, -1.628001950178158981E-16 ) ) ;
#1254 = DIRECTION ( 'NONE',  ( 3.032184104443271834E-30, 1.000000000000000000, 4.437342591868167759E-31 ) ) ;
#1255 = CARTESIAN_POINT ( 'NONE',  ( -4.857225732735059864E-14, 4.999999999999976907, -7.500000000000003553 ) ) ;
#1256 = AXIS2_PLACEMENT_3D ( 'NONE', #7873, #3869, #9180 ) ;
#1257 = VECTOR ( 'NONE', #20720, 1000.000000000000000 ) ;
#1258 = DIRECTION ( 'NONE',  ( -1.000000000000000000, 2.168404344971005170E-16, -1.203141491611682442E-30 ) ) ;
#1259 = VECTOR ( 'NONE', #901, 1000.000000000000000 ) ;
#1260 = DIRECTION ( 'NONE',  ( 1.000000000000000000, 0.000000000000000000, 0.000000000000000000 ) ) ;
#1261 = VECTOR ( 'NONE', #12249, 1000.000000000000000 ) ;
#1262 = ORIENTED_EDGE ( 'NONE', *, *, #10236, .T. ) ;
#1263 = COLOUR_RGB ( '', 0.31764706, 0.68627451, 0.89019608) ;
#1264 = PRESENTATION_STYLE_ASSIGNMENT (( #18908 ) ) ;
#1265 = CARTESIAN_POINT ( 'NONE',  ( 2.099999999999999645, 0.000000000000000000, -5.600000000000000533 ) ) ;
#1266 = CARTESIAN_POINT ( 'NONE',  ( -7.500000000000007105, -11.35410196624970780, 9.250000000000035527 ) ) ;
#1267 = ORIENTED_EDGE ( 'NONE', *, *, #2745, .T. ) ;
#1268 = EDGE_CURVE ( 'NONE', #6421, #12056, #9925, .T. ) ;
#1269 = EDGE_LOOP ( 'NONE', ( #6367, #10826, #1697, #13479 ) ) ;
#1270 = ORIENTED_EDGE ( 'NONE', *, *, #20922, .F. ) ;
#1271 = EDGE_CURVE ( 'NONE', #11689, #5606, #19039, .T. ) ;
#1272 = CARTESIAN_POINT ( 'NONE',  ( 4.165266963751715679, 2.049631966911993786, 3.550066703508900634 ) ) ;
#1273 = DIRECTION ( 'NONE',  ( 0.000000000000000000, 0.000000000000000000, 1.000000000000000000 ) ) ;
#1274 = AXIS2_PLACEMENT_3D ( 'NONE', #6348, #13400, #4804 ) ;
#1275 = VERTEX_POINT ( 'NONE', #11670 ) ;
#1276 = AXIS2_PLACEMENT_3D ( 'NONE', #16097, #15759, #12105 ) ;
#1277 = DIRECTION ( 'NONE',  ( -1.000000000000000000, -4.052314039881828472E-15, -1.387778780781436998E-15 ) ) ;
#1278 = CIRCLE ( 'NONE', #11789, 3.499999999999996003 ) ;
#1279 = DIRECTION ( 'NONE',  ( -0.7313537016191735685, 0.6819983600624951459, -3.923113172947598083E-16 ) ) ;
#1280 = CARTESIAN_POINT ( 'NONE',  ( 3.951447005078446484, -3.704664227300101143, 0.5833333333333329263 ) ) ;
#1281 = CIRCLE ( 'NONE', #14424, 0.2500000000000003331 ) ;
#1282 = CARTESIAN_POINT ( 'NONE',  ( -7.500000000000007105, 1.387778780781445676E-14, 6.249999999999992006 ) ) ;
#1283 = CARTESIAN_POINT ( 'NONE',  ( -2.500000000000002220, 3.061616997868386099E-16, -5.600000000000000533 ) ) ;
#1284 = B_SPLINE_CURVE_WITH_KNOTS ( 'NONE', 3,
 ( #1652, #6958, #21305, #12340, #20109, #21655 ),
 .UNSPECIFIED., .F., .F.,
 ( 4, 2, 4 ),
 ( 0.01103795673506155310, 0.01206113197427182565, 0.01308430721348209647 ),
 .UNSPECIFIED. ) ;
#1285 = CARTESIAN_POINT ( 'NONE',  ( -7.490313984279710624, -0.1442844712670970087, 7.566633644154755700 ) ) ;
#1286 = EDGE_CURVE ( 'NONE', #6388, #774, #23033, .T. ) ;
#1287 = CYLINDRICAL_SURFACE ( 'NONE', #4701, 0.5000000000000017764 ) ;
#1288 = DIRECTION ( 'NONE',  ( 0.000000000000000000, 0.000000000000000000, 1.000000000000000000 ) ) ;
#1289 = FACE_OUTER_BOUND ( 'NONE', #19754, .T. ) ;
#1290 = CARTESIAN_POINT ( 'NONE',  ( -6.938893903907228378E-14, 4.999999999999976907, -4.163336342344337027E-14 ) ) ;
#1291 = DIRECTION ( 'NONE',  ( -2.013525853228507892E-32, -6.902532920683810383E-31, 1.000000000000000000 ) ) ;
#1292 = AXIS2_PLACEMENT_3D ( 'NONE', #17237, #11834, #13607 ) ;
#1293 = CARTESIAN_POINT ( 'NONE',  ( 0.000000000000000000, 0.000000000000000000, -5.600000000000000533 ) ) ;
#1294 = AXIS2_PLACEMENT_3D ( 'NONE', #19329, #22516, #6859 ) ;
#1295 = ORIENTED_EDGE ( 'NONE', *, *, #18492, .F. ) ;
#1296 = TOROIDAL_SURFACE ( 'NONE', #11415, 6.500000000000000888, 0.5000000000000000000 ) ;
#1297 = ORIENTED_EDGE ( 'NONE', *, *, #12754, .F. ) ;
#1298 = CARTESIAN_POINT ( 'NONE',  ( 5.600000000000000533, 4.041451884327335264, -1.734723475976807094E-14 ) ) ;
#1300 = ORIENTED_EDGE ( 'NONE', *, *, #4213, .F. ) ;
#1299 = EDGE_LOOP ( 'NONE', ( #4669, #13365, #960, #3584 ) ) ;
#1301 = DIRECTION ( 'NONE',  ( -1.550910762415566494E-16, -1.000000000000000000, 8.135128085091684243E-31 ) ) ;
#1302 = DIRECTION ( 'NONE',  ( -4.190823558986625216E-31, 1.000000000000000000, -4.190823558986625216E-31 ) ) ;
#1303 = LINE ( 'NONE', #8350, #11618 ) ;
#1304 = AXIS2_PLACEMENT_3D ( 'NONE', #16015, #18033, #160 ) ;
#1305 = ORIENTED_EDGE ( 'NONE', *, *, #10538, .T. ) ;
#1306 = CONICAL_SURFACE ( 'NONE', #14454, 3.500000000000004441, 1.047197551196600296 ) ;
#1307 = LINE ( 'NONE', #9688, #8776 ) ;
#1308 = CIRCLE ( 'NONE', #3557, 0.7500000000000006661 ) ;
#1309 = CARTESIAN_POINT ( 'NONE',  ( -49.51923881554282048, 1.137615433949801247, 8.000000000000062172 ) ) ;
#1310 = CARTESIAN_POINT ( 'NONE',  ( -95.70000000000071338, 2.775557561562891351E-14, 1.000000000000070166 ) ) ;
#1311 = VECTOR ( 'NONE', #6045, 1000.000000000000114 ) ;
#1312 = CARTESIAN_POINT ( 'NONE',  ( -0.4634555469063579292, 1.750000000000002220, 4.749999999999999112 ) ) ;
#1313 = ADVANCED_FACE ( 'NONE', ( #988 ), #13453, .T. ) ;
#1314 = CARTESIAN_POINT ( 'NONE',  ( -87.15000000000064517, 5.607736497381665307E-14, -2.000000000000001332 ) ) ;
#1315 = PLANE ( 'NONE',  #14813 ) ;
#1316 = CARTESIAN_POINT ( 'NONE',  ( -7.499999999999992895, -5.999999999999987566, 6.249999999999992006 ) ) ;
#1317 = CARTESIAN_POINT ( 'NONE',  ( -4.182780094295433848, 0.7500000000000507372, -2.876053189442132396 ) ) ;
#1318 = ADVANCED_FACE ( 'NONE', ( #17075 ), #22512, .F. ) ;
#1319 = B_SPLINE_CURVE_WITH_KNOTS ( 'NONE', 3,
 ( #5797, #12433, #10558, #22484, #8680, #10012, #8012, #18956 ),
 .UNSPECIFIED., .F., .F.,
 ( 4, 2, 2, 4 ),
 ( 0.000000000000000000, 0.002450665683189824466, 0.003675998524784736699, 0.004901331366379648932 ),
 .UNSPECIFIED. ) ;
#1320 = LINE ( 'NONE', #19072, #6700 ) ;
#1321 = EDGE_CURVE ( 'NONE', #5639, #8147, #17136, .T. ) ;
#1322 = ORIENTED_EDGE ( 'NONE', *, *, #5382, .T. ) ;
#1323 = CONICAL_SURFACE ( 'NONE', #16330, 4.750000000000000888, 1.047197551196600074 ) ;
#1324 = ADVANCED_BREP_SHAPE_REPRESENTATION ( '', ( #5581, #22115 ), #19511 ) ;
#1325 = VECTOR ( 'NONE', #1887, 1000.000000000000000 ) ;
#1327 = ORIENTED_EDGE ( 'NONE', *, *, #19749, .F. ) ;
#1326 = ORIENTED_EDGE ( 'NONE', *, *, #21892, .F. ) ;
#1328 = UNCERTAINTY_MEASURE_WITH_UNIT (LENGTH_MEASURE( 1.000000000000000082E-05 ), #920, 'distance_accuracy_value', 'NONE');
#1330 = VERTEX_POINT ( 'NONE', #19844 ) ;
#1329 = VERTEX_POINT ( 'NONE', #16847 ) ;
#1331 = EDGE_LOOP ( 'NONE', ( #20654, #22644, #11760, #18194 ) ) ;
#1332 = CARTESIAN_POINT ( 'NONE',  ( 88.75737332930594903, -6.527605602963476805, 6.500000000000151879 ) ) ;
#1333 = DIRECTION ( 'NONE',  ( -1.144237745221811361E-17, 1.000000000000000000, -7.025792437124636392E-31 ) ) ;
#1334 = ADVANCED_FACE ( 'NONE', ( #20519 ), #639, .F. ) ;
#1335 = CARTESIAN_POINT ( 'NONE',  ( 88.75737332930594903, -13.02760560296348302, 6.000000000000130562 ) ) ;
#1336 = CARTESIAN_POINT ( 'NONE',  ( 10.50000000000000888, -0.5000000000000004441, 9.250000000000008882 ) ) ;
#1337 = CARTESIAN_POINT ( 'NONE',  ( -7.554637128289355630, -0.1201405311246572377, 7.453047528892588147 ) ) ;
#1338 = CARTESIAN_POINT ( 'NONE',  ( -6.000000000000143885, -2.000000000000043521, -8.000000000000035527 ) ) ;
#1339 = EDGE_CURVE ( 'NONE', #8929, #15576, #4500, .T. ) ;
#1340 = DIRECTION ( 'NONE',  ( 1.000000000000000000, 3.254448077276381206E-32, 1.066788928082016908E-26 ) ) ;
#1341 = CARTESIAN_POINT ( 'NONE',  ( 37.00000000000017053, 0.2500000000000002220, -10.43301270189217433 ) ) ;
#1342 = AXIS2_PLACEMENT_3D ( 'NONE', #958, #10123, #18822 ) ;
#1343 = CARTESIAN_POINT ( 'NONE',  ( 4.158806752148102248, -2.089318365061878069, 3.499999999999995115 ) ) ;
#1344 = CARTESIAN_POINT ( 'NONE',  ( -8.697224362268011433, -0.4999999999999970024, 6.250000000000033751 ) ) ;
#1345 = EDGE_CURVE ( 'NONE', #1131, #5232, #18083, .T. ) ;
#1346 = DIRECTION ( 'NONE',  ( 0.000000000000000000, 0.000000000000000000, -1.000000000000000000 ) ) ;
#1347 = EDGE_CURVE ( 'NONE', #5868, #17819, #1969, .T. ) ;
#1348 = DIRECTION ( 'NONE',  ( 2.220446049250313081E-16, -1.000000000000000000, 7.025792437124636392E-31 ) ) ;
#1349 = CARTESIAN_POINT ( 'NONE',  ( -50.65685424949274562, 0.5000000000000143219, -8.000000000000062172 ) ) ;
#1350 = ADVANCED_FACE ( 'NONE', ( #7920 ), #4263, .T. ) ;
#1351 = ORIENTED_EDGE ( 'NONE', *, *, #2302, .T. ) ;
#1353 = ORIENTED_EDGE ( 'NONE', *, *, #11369, .T. ) ;
#1352 = ORIENTED_EDGE ( 'NONE', *, *, #22036, .T. ) ;
#1354 = ORIENTED_EDGE ( 'NONE', *, *, #16873, .F. ) ;
#1355 = EDGE_LOOP ( 'NONE', ( #9247, #2066, #15136, #15479 ) ) ;
#1356 = EDGE_CURVE ( 'NONE', #8464, #7694, #5367, .T. ) ;
#1357 = ORIENTED_EDGE ( 'NONE', *, *, #4323, .T. ) ;
#1358 = EDGE_CURVE ( 'NONE', #10173, #15286, #5089, .T. ) ;
#1359 = DIRECTION ( 'NONE',  ( -1.000000000000000000, 0.000000000000000000, -1.066194817212772764E-26 ) ) ;
#1360 = EDGE_CURVE ( 'NONE', #10905, #8024, #13909, .T. ) ;
#1361 = AXIS2_PLACEMENT_3D ( 'NONE', #12480, #2122, #5209 ) ;
#1362 = DIRECTION ( 'NONE',  ( 0.000000000000000000, 3.469446951953619316E-15, 1.000000000000000000 ) ) ;
#1363 = ORIENTED_EDGE ( 'NONE', *, *, #15580, .F. ) ;
#1364 = DIRECTION ( 'NONE',  ( 1.000000000000000000, 0.000000000000000000, 0.000000000000000000 ) ) ;
#1365 = DIRECTION ( 'NONE',  ( -1.000000000000000000, 4.190823558986610327E-31, -1.733449886265890494E-32 ) ) ;
#1366 = STYLED_ITEM ( 'NONE', ( #22113 ), #21090 ) ;
#1367 = CARTESIAN_POINT ( 'NONE',  ( 4.000000000000004441, -1.549102112939114484, -5.442104661404057353 ) ) ;
#1368 = LINE ( 'NONE', #3251, #10465 ) ;
#1369 = PLANE ( 'NONE',  #20431 ) ;
#1370 = CARTESIAN_POINT ( 'NONE',  ( -6.959227686631209941, 36.00023952070644384, -18.50706566189541391 ) ) ;
#1371 = EDGE_CURVE ( 'NONE', #5959, #11179, #15659, .T. ) ;
#1372 = CARTESIAN_POINT ( 'NONE',  ( -0.9238745061264534986, -1.710161125106381963, 4.749999999999999112 ) ) ;
#1373 = DIRECTION ( 'NONE',  ( 0.000000000000000000, 9.769962616701412266E-15, 1.000000000000000000 ) ) ;
#1374 = EDGE_CURVE ( 'NONE', #6466, #18914, #19429, .T. ) ;
#1375 = AXIS2_PLACEMENT_3D ( 'NONE', #1590, #4999, #20901 ) ;
#1376 = CARTESIAN_POINT ( 'NONE',  ( -5.786576545576803454, 13.89610628501159795, -16.58192921595065883 ) ) ;
#1377 = CARTESIAN_POINT ( 'NONE',  ( -8.832214555408084422, -1.499999999999987343, 6.752214322824768189 ) ) ;
#1378 = ORIENTED_EDGE ( 'NONE', *, *, #10707, .F. ) ;
#1379 = FILL_AREA_STYLE ('',( #17353 ) ) ;
#1380 = CARTESIAN_POINT ( 'NONE',  ( 4.052424581287492167, 3.786734753434579215, 0.5771415817955150018 ) ) ;
#1381 = CARTESIAN_POINT ( 'NONE',  ( 4.630153689607049650, 0.000000000000000000, -3.469446951953614189E-15 ) ) ;
#1383 = ORIENTED_EDGE ( 'NONE', *, *, #22635, .F. ) ;
#1382 = EDGE_LOOP ( 'NONE', ( #8989, #21213, #23151, #14355 ) ) ;
#1384 = ORIENTED_EDGE ( 'NONE', *, *, #18533, .F. ) ;
#1385 = CARTESIAN_POINT ( 'NONE',  ( 4.175075985190096262, 2.060370777630112116, 3.568666869285570531 ) ) ;
#1386 = LINE ( 'NONE', #22918, #16285 ) ;
#1387 = CARTESIAN_POINT ( 'NONE',  ( 0.4637351970278817959, 1.750000000000001776, 4.749999999999999112 ) ) ;
#1388 = CARTESIAN_POINT ( 'NONE',  ( -10.49999999999996803, -6.938893903907228378E-15, 5.749999999999976907 ) ) ;
#1389 = CARTESIAN_POINT ( 'NONE',  ( 119.5756419024615838, -11.00000000000006573, -6.500000000000075495 ) ) ;
#1390 = CARTESIAN_POINT ( 'NONE',  ( 42.00000000000020606, 0.4999999999999865663, -0.4999999999999449329 ) ) ;
#1391 = DIRECTION ( 'NONE',  ( 0.6819983600624981435, -0.7313537016191709039, 0.000000000000000000 ) ) ;
#1392 = EDGE_CURVE ( 'NONE', #13556, #12774, #13038, .T. ) ;
#1393 = CARTESIAN_POINT ( 'NONE',  ( 0.000000000000000000, 0.000000000000000000, 0.000000000000000000 ) ) ;
#1394 = DIRECTION ( 'NONE',  ( 3.330669073875454830E-16, 0.000000000000000000, -1.000000000000000000 ) ) ;
#1395 = LINE ( 'NONE', #22932, #3517 ) ;
#1396 = TOROIDAL_SURFACE ( 'NONE', #14920, 1.300000000000000711, 0.5000000000000000000 ) ;
#1397 = CARTESIAN_POINT ( 'NONE',  ( 0.000000000000000000, -14.99999999999997513, -1.387778780781445676E-14 ) ) ;
#1398 = DIRECTION ( 'NONE',  ( 9.121204216617949000E-31, 1.000000000000000000, -6.982962677686261977E-15 ) ) ;
#1399 = EDGE_CURVE ( 'NONE', #12860, #8601, #3217, .T. ) ;
#1400 = CARTESIAN_POINT ( 'NONE',  ( -12.84999999999999964, 0.000000000000000000, 0.000000000000000000 ) ) ;
#1401 = ORIENTED_EDGE ( 'NONE', *, *, #12037, .T. ) ;
#1402 = ORIENTED_EDGE ( 'NONE', *, *, #14002, .F. ) ;
#1403 = CONICAL_SURFACE ( 'NONE', #9662, 5.371010071662839280, 1.221730476396037490 ) ;
#1404 = DIRECTION ( 'NONE',  ( 1.000000000000000000, 1.479114197289397135E-31, -7.395570986446975166E-31 ) ) ;
#1405 = VECTOR ( 'NONE', #13055, 1000.000000000000000 ) ;
#1407 = EDGE_LOOP ( 'NONE', ( #11723, #2320, #18772, #3662 ) ) ;
#1406 = ORIENTED_EDGE ( 'NONE', *, *, #11534, .F. ) ;
#1408 = CARTESIAN_POINT ( 'NONE',  ( 4.236525694536517506, -2.416953475386506067, -3.751298745799835022 ) ) ;
#1409 = ORIENTED_EDGE ( 'NONE', *, *, #4321, .T. ) ;
#1410 = SURFACE_STYLE_USAGE ( .BOTH. , #17513 ) ;
#1411 = FACE_OUTER_BOUND ( 'NONE', #1407, .T. ) ;
#1412 = AXIS2_PLACEMENT_3D ( 'NONE', #8513, #19100, #13917 ) ;
#1413 = ORIENTED_EDGE ( 'NONE', *, *, #10933, .T. ) ;
#1414 = CARTESIAN_POINT ( 'NONE',  ( -64.00000000000045475, 6.245004513516505540E-14, -1.999999999999974021 ) ) ;
#1415 = DIRECTION ( 'NONE',  ( -1.331202777560457422E-30, -1.000000000000000000, 7.395570986446985676E-31 ) ) ;
#1416 = CARTESIAN_POINT ( 'NONE',  ( 2.775557561562891351E-14, 11.00000000000000000, -9.999999999999968026 ) ) ;
#1417 = PRODUCT_DEFINITION_SHAPE ( 'NONE', 'NONE',  #23276 ) ;
#1418 = CIRCLE ( 'NONE', #13068, 2.550000000000010481 ) ;
#1419 = DIRECTION ( 'NONE',  ( -1.064962222048364933E-26, 0.000000000000000000, -1.000000000000000000 ) ) ;
#1420 = AXIS2_PLACEMENT_3D ( 'NONE', #19154, #10205, #5034 ) ;
#1421 = DIRECTION ( 'NONE',  ( -3.885780586188016830E-16, -4.437342591868156373E-31, 1.000000000000000000 ) ) ;
#1422 = DIRECTION ( 'NONE',  ( -2.013525853228507892E-32, -6.902532920683810383E-31, 1.000000000000000000 ) ) ;
#1423 = AXIS2_PLACEMENT_3D ( 'NONE', #8985, #5458, #16483 ) ;
#1424 = CARTESIAN_POINT ( 'NONE',  ( -50.65685424949280247, 1.387778780781445676E-14, 8.000000000000090594 ) ) ;
#1426 = CIRCLE ( 'NONE', #20211, 2.499999999999993783 ) ;
#1425 = APPLICATION_CONTEXT ( 'automotive_design' ) ;
#1427 = ORIENTED_EDGE ( 'NONE', *, *, #5079, .T. ) ;
#1428 = AXIS2_PLACEMENT_3D ( 'NONE', #13780, #1092, #17412 ) ;
#1429 = APPLICATION_PROTOCOL_DEFINITION ( 'draft international standard', 'automotive_design', 1998, #7443 ) ;
#1431 = ORIENTED_EDGE ( 'NONE', *, *, #2761, .T. ) ;
#1430 = VERTEX_POINT ( 'NONE', #15434 ) ;
#1432 = ADVANCED_FACE ( 'NONE', ( #22976 ), #12015, .F. ) ;
#1433 = VERTEX_POINT ( 'NONE', #6398 ) ;
#1435 = ORIENTED_EDGE ( 'NONE', *, *, #20235, .F. ) ;
#1434 = ORIENTED_EDGE ( 'NONE', *, *, #488, .F. ) ;
#1436 = CARTESIAN_POINT ( 'NONE',  ( 58.85734743794750301, 0.7537990605245015185, -5.999999999999880096 ) ) ;
#1437 = FACE_OUTER_BOUND ( 'NONE', #5827, .T. ) ;
#1438 = FILL_AREA_STYLE_COLOUR ( '', #1263 ) ;
#1439 = LINE ( 'NONE', #21221, #3812 ) ;
#1440 = CARTESIAN_POINT ( 'NONE',  ( 80.49335071782263640, -7.708908342713538531, 6.500000000000033751 ) ) ;
#1441 = AXIS2_PLACEMENT_3D ( 'NONE', #19500, #6925, #1618 ) ;
#1442 = DIRECTION ( 'NONE',  ( -2.220446049250313081E-16, 1.000000000000000000, -7.025792437124636392E-31 ) ) ;
#1443 = CARTESIAN_POINT ( 'NONE',  ( 7.499999999999978684, -12.60977222864647196, 9.250000000000049738 ) ) ;
#1444 = VECTOR ( 'NONE', #442, 1000.000000000000000 ) ;
#1445 = PLANE ( 'NONE',  #551 ) ;
#1446 = CARTESIAN_POINT ( 'NONE',  ( 7.000000000000006217, -5.999999999999981348, 10.24999999999998224 ) ) ;
#1447 = AXIS2_PLACEMENT_3D ( 'NONE', #6198, #17344, #1252 ) ;
#1448 = CARTESIAN_POINT ( 'NONE',  ( -3.349226789952745698, -2.685125164760777672, -0.2236248678335490125 ) ) ;
#1449 = CARTESIAN_POINT ( 'NONE',  ( 4.113620667976075396, -1.749999999999998002, -2.375000000000002220 ) ) ;
#1450 = CARTESIAN_POINT ( 'NONE',  ( 5.261076337303417283, 1.454929939081818002, 0.3875484812921120015 ) ) ;
#1451 = DIRECTION ( 'NONE',  ( 0.000000000000000000, 1.000000000000000000, -0.000000000000000000 ) ) ;
#1452 = CARTESIAN_POINT ( 'NONE',  ( 0.000000000000000000, 3.031088913245528982, -1.750000000000001554 ) ) ;
#1453 = DIRECTION ( 'NONE',  ( 3.885780586188016830E-16, 4.437342591868156373E-31, -1.000000000000000000 ) ) ;
#1454 = ORIENTED_EDGE ( 'NONE', *, *, #13692, .F. ) ;
#1455 = EDGE_CURVE ( 'NONE', #5339, #2694, #13565, .T. ) ;
#1457 = ORIENTED_EDGE ( 'NONE', *, *, #11127, .F. ) ;
#1456 = ORIENTED_EDGE ( 'NONE', *, *, #16684, .T. ) ;
#1458 = EDGE_CURVE ( 'NONE', #4755, #10141, #22619, .T. ) ;
#1459 = ORIENTED_EDGE ( 'NONE', *, *, #2823, .F. ) ;
#1460 = AXIS2_PLACEMENT_3D ( 'NONE', #13839, #22554, #6324 ) ;
#1461 = EDGE_LOOP ( 'NONE', ( #12981, #897, #19929, #16564 ) ) ;
#1462 = CIRCLE ( 'NONE', #22131, 4.366025403784456138 ) ;
#1463 = ORIENTED_EDGE ( 'NONE', *, *, #14109, .T. ) ;
#1464 = ORIENTED_EDGE ( 'NONE', *, *, #21499, .F. ) ;
#1465 = CARTESIAN_POINT ( 'NONE',  ( 2.773872027545001791E-14, 1.041826426137094221E-16, 2.500000000000000000 ) ) ;
#1466 = EDGE_CURVE ( 'NONE', #16593, #10367, #6244, .T. ) ;
#1467 = EDGE_CURVE ( 'NONE', #15040, #9447, #5099, .T. ) ;
#1468 = CARTESIAN_POINT ( 'NONE',  ( -12.84999999999999964, -12.50000000000006928, 6.938893903907228378E-14 ) ) ;
#1469 = ORIENTED_EDGE ( 'NONE', *, *, #108, .F. ) ;
#1470 = CARTESIAN_POINT ( 'NONE',  ( -64.00000000000038369, -3.200000000000081446, -2.000000000000029310 ) ) ;
#1471 = EDGE_CURVE ( 'NONE', #21722, #18197, #11793, .T. ) ;
#1472 =( GEOMETRIC_REPRESENTATION_CONTEXT ( 3 ) GLOBAL_UNCERTAINTY_ASSIGNED_CONTEXT ( ( #3709 ) ) GLOBAL_UNIT_ASSIGNED_CONTEXT ( ( #13921, #3112, #6999 ) ) REPRESENTATION_CONTEXT ( 'NONE', 'WORKASPACE' ) );
#1473 = CARTESIAN_POINT ( 'NONE',  ( 2.805705207896037390, -3.226868319750231695, -3.503898532754383233 ) ) ;
#1474 = PLANE ( 'NONE',  #8000 ) ;
#1475 = CARTESIAN_POINT ( 'NONE',  ( 4.071447262713884463, -2.020725942163709377, 3.500000000000003109 ) ) ;
#1476 = DIRECTION ( 'NONE',  ( 0.000000000000000000, 0.000000000000000000, -1.000000000000000000 ) ) ;
#1477 = B_SPLINE_CURVE_WITH_KNOTS ( 'NONE', 3,
 ( #3275, #1280, #2918, #21039, #3037 ),
 .UNSPECIFIED., .F., .F.,
 ( 4, 1, 4 ),
 ( 0.000000000000000000, 0.002020725942163690073, 0.004041451884327380145 ),
 .UNSPECIFIED. ) ;
#1478 = DIRECTION ( 'NONE',  ( 1.000000000000000000, 4.440892098500626162E-16, -5.551115123125782702E-16 ) ) ;
#1479 = DIRECTION ( 'NONE',  ( -1.000000000000000000, 0.000000000000000000, 0.000000000000000000 ) ) ;
#1480 = DIRECTION ( 'NONE',  ( -3.070652698126927723E-17, -1.000000000000000000, 4.167305704548413124E-17 ) ) ;
#1481 = DIRECTION ( 'NONE',  ( 0.000000000000000000, -4.190823558986610327E-31, 1.000000000000000000 ) ) ;
#1482 = AXIS2_PLACEMENT_3D ( 'NONE', #12903, #16644, #3954 ) ;
#1483 = DIRECTION ( 'NONE',  ( -1.333893503340774882E-15, -2.778352770573747380E-17, -1.000000000000000000 ) ) ;
#1484 = DIRECTION ( 'NONE',  ( -5.551115123125796261E-17, 0.000000000000000000, 1.000000000000000000 ) ) ;
#1485 = EDGE_CURVE ( 'NONE', #13386, #1178, #9993, .T. ) ;
#1486 = ORIENTED_EDGE ( 'NONE', *, *, #426, .F. ) ;
#1487 = EDGE_CURVE ( 'NONE', #12036, #18303, #13685, .T. ) ;
#1488 = ADVANCED_FACE ( 'NONE', ( #15553 ), #13794, .F. ) ;
#1489 = CARTESIAN_POINT ( 'NONE',  ( 3.973514160553464514, 3.435084588004195805, -1.181876024140321224 ) ) ;
#1490 = CARTESIAN_POINT ( 'NONE',  ( -89.70000000000055707, -3.200000000000105427, -1.999999999999946265 ) ) ;
#1491 = CONICAL_SURFACE ( 'NONE', #1847, 4.000000000000000000, 1.047197551196595855 ) ;
#1493 = EDGE_LOOP ( 'NONE', ( #12083, #18786, #20478, #1434 ) ) ;
#1492 = ORIENTED_EDGE ( 'NONE', *, *, #10315, .F. ) ;
#1494 =( GEOMETRIC_REPRESENTATION_CONTEXT ( 3 ) GLOBAL_UNCERTAINTY_ASSIGNED_CONTEXT ( ( #7707 ) ) GLOBAL_UNIT_ASSIGNED_CONTEXT ( ( #8490, #19540, #17780 ) ) REPRESENTATION_CONTEXT ( 'NONE', 'WORKASPACE' ) );
#1495 = VERTEX_POINT ( 'NONE', #1440 ) ;
#1497 = EDGE_LOOP ( 'NONE', ( #20808, #7884, #3817, #2556 ) ) ;
#1496 = EDGE_CURVE ( 'NONE', #4163, #4944, #19088, .T. ) ;
#1498 = ORIENTED_EDGE ( 'NONE', *, *, #3492, .T. ) ;
#1499 = CARTESIAN_POINT ( 'NONE',  ( -7.000000000000020428, -5.999999999999981348, 10.74999999999996803 ) ) ;
#1500 = CARTESIAN_POINT ( 'NONE',  ( 29.00000000029184832, 16.99999999900385461, -25.50000000000000355 ) ) ;
#1501 = EDGE_CURVE ( 'NONE', #20416, #635, #236, .T. ) ;
#1502 = DIRECTION ( 'NONE',  ( 1.091943820671237506E-16, -0.7904150521752423275, 0.6125716654358156488 ) ) ;
#1503 = FACE_OUTER_BOUND ( 'NONE', #18223, .T. ) ;
#1504 = LINE ( 'NONE', #8453, #19242 ) ;
#1505 = ORIENTED_EDGE ( 'NONE', *, *, #611, .T. ) ;
#1506 = CARTESIAN_POINT ( 'NONE',  ( -2.700000000000119194, 1.999999999999967137, -8.000000000000007105 ) ) ;
#1507 = CYLINDRICAL_SURFACE ( 'NONE', #1441, 2.549999999999997158 ) ;
#1508 = AXIS2_PLACEMENT_3D ( 'NONE', #5115, #8531, #3590 ) ;
#1509 = CARTESIAN_POINT ( 'NONE',  ( -7.132286784435581950, -0.4236497315829815813, 8.470912490188249322 ) ) ;
#1510 = DIRECTION ( 'NONE',  ( 1.000000000000000000, -0.000000000000000000, -0.000000000000000000 ) ) ;
#1511 = DIRECTION ( 'NONE',  ( 0.7313537016191745677, 0.6819983600624940356, 1.072890437865584285E-16 ) ) ;
#1512 = CARTESIAN_POINT ( 'NONE',  ( 25.00000000000001066, 0.2500000000000002220, -17.00000000000001066 ) ) ;
#1513 = CARTESIAN_POINT ( 'NONE',  ( 7.595478965369728108, -2.023942297479887742, 8.489833260407438686 ) ) ;
#1514 = DIRECTION ( 'NONE',  ( -1.000000000000000000, 4.615739097524200579E-16, 1.134196829589820086E-15 ) ) ;
#1515 = CARTESIAN_POINT ( 'NONE',  ( 0.1404048886732169876, 4.699864953788106092, -3.686887068327049377 ) ) ;
#1516 = DIRECTION ( 'NONE',  ( -1.927470528863118556E-16, 1.000000000000000000, 0.000000000000000000 ) ) ;
#1517 = DIRECTION ( 'NONE',  ( 2.168404344971017743E-16, 1.000000000000000000, -6.982962677686261977E-15 ) ) ;
#1518 = ORIENTED_EDGE ( 'NONE', *, *, #20201, .T. ) ;
#1519 = TOROIDAL_SURFACE ( 'NONE', #21814, 6.700000000000001066, 0.5000000000000000000 ) ;
#1520 = VERTEX_POINT ( 'NONE', #10375 ) ;
#1521 = ORIENTED_EDGE ( 'NONE', *, *, #13820, .F. ) ;
#1522 = EDGE_CURVE ( 'NONE', #22506, #18271, #8616, .T. ) ;
#1523 = FACE_OUTER_BOUND ( 'NONE', #22735, .T. ) ;
#1525 = ORIENTED_EDGE ( 'NONE', *, *, #5225, .T. ) ;
#1524 = EDGE_LOOP ( 'NONE', ( #1663, #9843, #66, #6122 ) ) ;
#1526 = FACE_OUTER_BOUND ( 'NONE', #8749, .T. ) ;
#1527 = CARTESIAN_POINT ( 'NONE',  ( 24.99999999999999645, 0.2499999999999863443, -19.00000000000001421 ) ) ;
#1528 = EDGE_CURVE ( 'NONE', #11543, #15515, #17880, .T. ) ;
#1529 = DIRECTION ( 'NONE',  ( 0.6819983600625074693, -0.7313537016191621332, 1.110084618464482116E-16 ) ) ;
#1530 = DIRECTION ( 'NONE',  ( -1.000000000000000000, 0.000000000000000000, -0.000000000000000000 ) ) ;
#1531 = ORIENTED_EDGE ( 'NONE', *, *, #16518, .F. ) ;
#1532 = FACE_OUTER_BOUND ( 'NONE', #21083, .T. ) ;
#1533 = DIRECTION ( 'NONE',  ( 1.000000000000000000, 0.000000000000000000, 0.000000000000000000 ) ) ;
#1534 = DIRECTION ( 'NONE',  ( -1.000000000000000000, 0.000000000000000000, 0.000000000000000000 ) ) ;
#1535 = CARTESIAN_POINT ( 'NONE',  ( -7.473326079327797800, -13.84852298796451464, 7.598194856234270489 ) ) ;
#1536 = CARTESIAN_POINT ( 'NONE',  ( 37.18301270189237329, 10.90849364905388619, -2.475480947161653233 ) ) ;
#1537 = AXIS2_PLACEMENT_3D ( 'NONE', #19881, #3750, #9051 ) ;
#1538 = CARTESIAN_POINT ( 'NONE',  ( 2.000000000000029310, 3.464101615137740175, 0.000000000000000000 ) ) ;
#1539 = DIRECTION ( 'NONE',  ( 2.013525853228507892E-32, 6.902532920683810383E-31, -1.000000000000000000 ) ) ;
#1540 = LINE ( 'NONE', #8714, #5955 ) ;
#1541 = EDGE_LOOP ( 'NONE', ( #19704, #15907, #14735, #4989 ) ) ;
#1542 = DIRECTION ( 'NONE',  ( 9.714451465470131562E-16, -1.000000000000000000, -1.334219193460660770E-15 ) ) ;
#1544 = ORIENTED_EDGE ( 'NONE', *, *, #20662, .F. ) ;
#1543 = ORIENTED_EDGE ( 'NONE', *, *, #22186, .F. ) ;
#1545 = ORIENTED_EDGE ( 'NONE', *, *, #22875, .F. ) ;
#1547 = VERTEX_POINT ( 'NONE', #5448 ) ;
#1546 = VERTEX_POINT ( 'NONE', #12368 ) ;
#1548 = VECTOR ( 'NONE', #20577, 1000.000000000000000 ) ;
#1549 = CIRCLE ( 'NONE', #7564, 0.5000000000000038858 ) ;
#1550 = VERTEX_POINT ( 'NONE', #10840 ) ;
#1551 = CARTESIAN_POINT ( 'NONE',  ( -89.70000000000064233, 5.551115123125782702E-14, -2.000000000000001776 ) ) ;
#1552 = DIRECTION ( 'NONE',  ( 1.331202777560457422E-30, 1.000000000000000000, -7.395570986446985676E-31 ) ) ;
#1553 = CARTESIAN_POINT ( 'NONE',  ( 82.19834661797897013, -5.880524088665628923, 6.500000000000151879 ) ) ;
#1554 = DIRECTION ( 'NONE',  ( -5.551115123561405253E-17, -1.000000000000000000, -2.256980353643891447E-27 ) ) ;
#1555 = CARTESIAN_POINT ( 'NONE',  ( -47.47487373415324186, 4.018019484660559471, 8.000000000000062172 ) ) ;
#1556 = DIRECTION ( 'NONE',  ( 0.000000000000000000, 0.000000000000000000, 1.000000000000000000 ) ) ;
#1557 = DIRECTION ( 'NONE',  ( -1.550910762415566494E-16, -1.000000000000000000, 8.135128085091684243E-31 ) ) ;
#1558 = CYLINDRICAL_SURFACE ( 'NONE', #19515, 2.499999999999993783 ) ;
#1559 = DIRECTION ( 'NONE',  ( -4.190823558986625216E-31, 1.000000000000000000, -4.190823558986625216E-31 ) ) ;
#1560 = DIRECTION ( 'NONE',  ( 5.551115123125733398E-17, 0.000000000000000000, -1.000000000000000000 ) ) ;
#1561 = DIRECTION ( 'NONE',  ( -4.190823558986625216E-31, 1.000000000000000000, -4.190823558986625216E-31 ) ) ;
#1562 = CYLINDRICAL_SURFACE ( 'NONE', #18135, 0.5000000000000022204 ) ;
#1563 = ADVANCED_FACE ( 'NONE', ( #19908 ), #16365, .T. ) ;
#1564 = DIRECTION ( 'NONE',  ( 0.000000000000000000, 0.000000000000000000, 1.000000000000000000 ) ) ;
#1565 = CARTESIAN_POINT ( 'NONE',  ( 2.999999999999999556, -1.685411297769503192E-31, 2.499999999999990674 ) ) ;
#1566 = AXIS2_PLACEMENT_3D ( 'NONE', #17345, #1253, #8430 ) ;
#1567 = DIRECTION ( 'NONE',  ( 3.885780586188016830E-16, 4.437342591868156373E-31, -1.000000000000000000 ) ) ;
#1568 = PLANE ( 'NONE',  #3642 ) ;
#1569 = ORIENTED_EDGE ( 'NONE', *, *, #7673, .F. ) ;
#1571 = VERTEX_POINT ( 'NONE', #7326 ) ;
#1570 = ORIENTED_EDGE ( 'NONE', *, *, #9831, .F. ) ;
#1572 = EDGE_LOOP ( 'NONE', ( #18166, #10366, #15393, #12226, #22817 ) ) ;
#1573 = ORIENTED_EDGE ( 'NONE', *, *, #2157, .F. ) ;
#1574 = EDGE_LOOP ( 'NONE', ( #5344, #16025, #6543, #19081 ) ) ;
#1575 = AXIS2_PLACEMENT_3D ( 'NONE', #22054, #20406, #22400 ) ;
#1576 = ORIENTED_EDGE ( 'NONE', *, *, #15133, .F. ) ;
#1577 = CARTESIAN_POINT ( 'NONE',  ( 2.918498775983380256E-10, -9.961476088449217059E-10, -26.00000000000000000 ) ) ;
#1578 = AXIS2_PLACEMENT_3D ( 'NONE', #16932, #6256, #843 ) ;
#1579 = AXIS2_PLACEMENT_3D ( 'NONE', #17020, #4198, #13042 ) ;
#1580 = LINE ( 'NONE', #10636, #7257 ) ;
#1581 = ORIENTED_EDGE ( 'NONE', *, *, #20471, .T. ) ;
#1582 = CARTESIAN_POINT ( 'NONE',  ( 42.00000000000012079, 2.999999999999999112, -12.49999999999999645 ) ) ;
#1583 = CIRCLE ( 'NONE', #2335, 12.14055452724117856 ) ;
#1584 = DIRECTION ( 'NONE',  ( 0.000000000000000000, 0.000000000000000000, -1.000000000000000000 ) ) ;
#1585 = ADVANCED_FACE ( 'NONE', ( #14263 ), #17498, .T. ) ;
#1586 = CARTESIAN_POINT ( 'NONE',  ( -6.245004513516505540E-14, -4.862606272033144883, -3.745885042887461935 ) ) ;
#1587 = CARTESIAN_POINT ( 'NONE',  ( 77.42435809754145737, -6.499999999999811706, -6.499999999999984901 ) ) ;
#1588 = CYLINDRICAL_SURFACE ( 'NONE', #22687, 2.550000000000010481 ) ;
#1589 = LINE ( 'NONE', #13077, #14723 ) ;
#1590 = CARTESIAN_POINT ( 'NONE',  ( 0.000000000000000000, 0.000000000000000000, 0.000000000000000000 ) ) ;
#1591 = ADVANCED_FACE ( 'NONE', ( #21452 ), #10724, .T. ) ;
#1592 = CARTESIAN_POINT ( 'NONE',  ( 0.3126073911695753660, -2.020725942163847932, -3.499999999999975131 ) ) ;
#1593 = CIRCLE ( 'NONE', #6099, 6.249999999999992006 ) ;
#1594 = CARTESIAN_POINT ( 'NONE',  ( 3.646393709166112718, 1.750000000000001998, 3.184260831324768226 ) ) ;
#1595 = CYLINDRICAL_SURFACE ( 'NONE', #10383, 0.5000000000000000000 ) ;
#1596 = ORIENTED_EDGE ( 'NONE', *, *, #20698, .F. ) ;
#1597 = EDGE_CURVE ( 'NONE', #20279, #8964, #13375, .T. ) ;
#1598 = CARTESIAN_POINT ( 'NONE',  ( 12.84999999999997300, -0.5000000000000004441, -6.249999999999963585 ) ) ;
#1599 = LINE ( 'NONE', #16169, #12664 ) ;
#1600 = VECTOR ( 'NONE', #21371, 1000.000000000000000 ) ;
#1601 = EDGE_CURVE ( 'NONE', #8927, #10359, #20790, .T. ) ;
#1603 = EDGE_LOOP ( 'NONE', ( #13242, #14531, #7061, #6609 ) ) ;
#1602 = ORIENTED_EDGE ( 'NONE', *, *, #4180, .F. ) ;
#1604 = CIRCLE ( 'NONE', #3842, 0.5000000000000038858 ) ;
#1605 = ADVANCED_FACE ( 'NONE', ( #9075 ), #23102, .F. ) ;
#1606 = CIRCLE ( 'NONE', #8742, 6.249999999999992006 ) ;
#1607 = ORIENTED_EDGE ( 'NONE', *, *, #14971, .F. ) ;
#1608 = ORIENTED_EDGE ( 'NONE', *, *, #15687, .F. ) ;
#1609 = PRODUCT_DEFINITION_SHAPE ( 'NONE', 'NONE',  #17672 ) ;
#1610 = ORIENTED_EDGE ( 'NONE', *, *, #10575, .T. ) ;
#1611 = CARTESIAN_POINT ( 'NONE',  ( 80.15235153779146060, -8.074585193523137860, 6.000000000000109246 ) ) ;
#1612 = DIRECTION ( 'NONE',  ( 1.550910762415566494E-16, 1.000000000000000000, -8.135128085091684243E-31 ) ) ;
#1613 = FACE_OUTER_BOUND ( 'NONE', #15280, .T. ) ;
#1614 = CARTESIAN_POINT ( 'NONE',  ( 77.42435809754135789, -10.99999999999981526, 6.500000000000123457 ) ) ;
#1615 = EDGE_CURVE ( 'NONE', #16004, #5080, #8970, .T. ) ;
#1616 = ADVANCED_FACE ( 'NONE', ( #19674 ), #7208, .T. ) ;
#1617 = LINE ( 'NONE', #19377, #10224 ) ;
#1618 = DIRECTION ( 'NONE',  ( 0.000000000000000000, 6.802837160693368935E-15, 1.000000000000000000 ) ) ;
#1619 = DIRECTION ( 'NONE',  ( 0.000000000000000000, 0.000000000000000000, 1.000000000000000000 ) ) ;
#1620 = VECTOR ( 'NONE', #8184, 1000.000000000000000 ) ;
#1622 = ADVANCED_FACE ( 'NONE', ( #19551 ), #8105, .T. ) ;
#1621 = VECTOR ( 'NONE', #16837, 1000.000000000000000 ) ;
#1623 = CARTESIAN_POINT ( 'NONE',  ( -5.484827557301438894, -1.325747111984083793, 0.000000000000000000 ) ) ;
#1624 = CARTESIAN_POINT ( 'NONE',  ( 37.73505106183036162, 10.99999999999229061, -10.73505106183359104 ) ) ;
#1625 = LINE ( 'NONE', #7049, #5406 ) ;
#1626 = PLANE ( 'NONE',  #11219 ) ;
#1627 =( LENGTH_UNIT ( ) NAMED_UNIT ( * ) SI_UNIT ( .MILLI., .METRE. ) );
#1628 = EDGE_CURVE ( 'NONE', #14201, #16629, #12993, .T. ) ;
#1629 = CARTESIAN_POINT ( 'NONE',  ( -8.660254037844428154, 4.689110867544629357, -1.387778780781445676E-14 ) ) ;
#1630 = LINE ( 'NONE', #8813, #3292 ) ;
#1631 = ORIENTED_EDGE ( 'NONE', *, *, #653, .F. ) ;
#1632 = EDGE_CURVE ( 'NONE', #15165, #21891, #10736, .T. ) ;
#1633 = AXIS2_PLACEMENT_3D ( 'NONE', #19620, #5400, #15962 ) ;
#1634 = AXIS2_PLACEMENT_3D ( 'NONE', #16389, #23134, #5714 ) ;
#1635 = ORIENTED_EDGE ( 'NONE', *, *, #1374, .F. ) ;
#1636 = EDGE_CURVE ( 'NONE', #7030, #18641, #5864, .T. ) ;
#1637 = AXIS2_PLACEMENT_3D ( 'NONE', #21705, #18178, #9458 ) ;
#1638 = AXIS2_PLACEMENT_3D ( 'NONE', #19755, #13874, #17507 ) ;
#1639 = CIRCLE ( 'NONE', #2014, 2.500000000000000000 ) ;
#1640 = STYLED_ITEM ( 'NONE', ( #13684 ), #13034 ) ;
#1642 = VERTEX_POINT ( 'NONE', #5793 ) ;
#1641 = ORIENTED_EDGE ( 'NONE', *, *, #10677, .T. ) ;
#1643 = CARTESIAN_POINT ( 'NONE',  ( 1.243802165048362607, -3.900692638707722093, -3.223146290109814682 ) ) ;
#1644 = FACE_OUTER_BOUND ( 'NONE', #14527, .T. ) ;
#1645 = EDGE_CURVE ( 'NONE', #10770, #2913, #600, .T. ) ;
#1646 = DIRECTION ( 'NONE',  ( 4.190823558986625216E-31, -1.000000000000000000, 4.190823558986625216E-31 ) ) ;
#1647 = CARTESIAN_POINT ( 'NONE',  ( 22.49999999999999645, 4.250000000000031974, -2.081668171172168513E-14 ) ) ;
#1648 = EDGE_CURVE ( 'NONE', #15365, #9160, #13753, .T. ) ;
#1649 = EDGE_LOOP ( 'NONE', ( #1326, #5753 ) ) ;
#1650 = DIRECTION ( 'NONE',  ( 2.013525853228508439E-32, 6.779273404243028164E-31, -1.000000000000000000 ) ) ;
#1651 = CARTESIAN_POINT ( 'NONE',  ( 4.071447262713884463, -2.020725942163695166, -3.500000000000000444 ) ) ;
#1652 = CARTESIAN_POINT ( 'NONE',  ( 0.3126073911696447549, 2.020725942163688504, -3.499999999999996003 ) ) ;
#1653 = CARTESIAN_POINT ( 'NONE',  ( 2.499999999999960476, 4.500000000000017764, -18.75000000000002132 ) ) ;
#1654 = CARTESIAN_POINT ( 'NONE',  ( 25.00000000000000355, 2.000000000000001776, -0.2500000000000002220 ) ) ;
#1655 = VECTOR ( 'NONE', #17115, 1000.000000000000000 ) ;
#1656 = DIRECTION ( 'NONE',  ( -1.000000000000000000, 4.190823558986610327E-31, -1.733449886265890494E-32 ) ) ;
#1657 = CARTESIAN_POINT ( 'NONE',  ( -12.85000000000001386, -14.00000000000007105, 5.551115123125782702E-14 ) ) ;
#1658 = CARTESIAN_POINT ( 'NONE',  ( 37.68301270189240171, 11.00000000000000533, -2.499999999999975575 ) ) ;
#1659 = EDGE_CURVE ( 'NONE', #5612, #5080, #16736, .T. ) ;
#1660 = AXIS2_PLACEMENT_3D ( 'NONE', #8212, #6447, #1159 ) ;
#1661 = DIRECTION ( 'NONE',  ( 1.000000000000000000, 1.479114197289388027E-30, -2.013525853228518840E-32 ) ) ;
#1662 = DIRECTION ( 'NONE',  ( 0.000000000000000000, 0.000000000000000000, 1.000000000000000000 ) ) ;
#1663 = ORIENTED_EDGE ( 'NONE', *, *, #15877, .T. ) ;
#1664 = DIRECTION ( 'NONE',  ( 0.000000000000000000, 4.163336342344337027E-17, -1.000000000000000000 ) ) ;
#1666 = ORIENTED_EDGE ( 'NONE', *, *, #20945, .F. ) ;
#1665 = VERTEX_POINT ( 'NONE', #15051 ) ;
#1667 = EDGE_LOOP ( 'NONE', ( #61, #23206, #12396, #397 ) ) ;
#1669 = VERTEX_POINT ( 'NONE', #11524 ) ;
#1668 = ORIENTED_EDGE ( 'NONE', *, *, #16268, .F. ) ;
#1670 = AXIS2_PLACEMENT_3D ( 'NONE', #6502, #15199, #22268 ) ;
#1671 = AXIS2_PLACEMENT_3D ( 'NONE', #14122, #21310, #19533 ) ;
#1672 = CARTESIAN_POINT ( 'NONE',  ( -67.28510754798018922, 1.387778780781445676E-14, 12.22107821754958579 ) ) ;
#1673 = AXIS2_PLACEMENT_3D ( 'NONE', #18535, #5961, #3950 ) ;
#1674 = CARTESIAN_POINT ( 'NONE',  ( -3.999999999708153453, 38.99999999900385461, -15.99999999999999289 ) ) ;
#1675 = SURFACE_STYLE_USAGE ( .BOTH. , #15775 ) ;
#1676 = DIRECTION ( 'NONE',  ( -3.241725282392603095E-30, -1.000000000000000000, 2.218671295934100958E-31 ) ) ;
#1677 = DIRECTION ( 'NONE',  ( -8.438582421954109416E-32, 0.000000000000000000, -1.000000000000000000 ) ) ;
#1678 = DIRECTION ( 'NONE',  ( 7.860214984770699307E-18, -1.409037165336591006E-16, -1.000000000000000000 ) ) ;
#1679 = AXIS2_PLACEMENT_3D ( 'NONE', #13346, #7927, #22169 ) ;
#1680 = CARTESIAN_POINT ( 'NONE',  ( 4.484612144975566039, -0.7499999999999384936, -2.618262478605820398 ) ) ;
#1681 = EDGE_CURVE ( 'NONE', #8658, #12443, #16806, .T. ) ;
#1682 = DIRECTION ( 'NONE',  ( 1.387778780781437314E-14, 0.000000000000000000, -1.000000000000000000 ) ) ;
#1683 = FACE_OUTER_BOUND ( 'NONE', #1741, .T. ) ;
#1684 = DIRECTION ( 'NONE',  ( -2.013525853228507892E-32, -6.902532920683810383E-31, 1.000000000000000000 ) ) ;
#1685 = CARTESIAN_POINT ( 'NONE',  ( 2.804994570502168827, 3.229033611042460006, -3.526374918436841366 ) ) ;
#1686 = CARTESIAN_POINT ( 'NONE',  ( 12.84999999999997300, -12.50000000000006928, 5.551115123125782702E-14 ) ) ;
#1687 = EDGE_CURVE ( 'NONE', #19077, #4132, #10111, .T. ) ;
#1688 = LINE ( 'NONE', #5330, #1013 ) ;
#1689 = CIRCLE ( 'NONE', #7335, 0.5000000000000019984 ) ;
#1690 = DIRECTION ( 'NONE',  ( 9.121204216617949000E-31, 1.000000000000000000, -6.982962677686261977E-15 ) ) ;
#1691 = CARTESIAN_POINT ( 'NONE',  ( -4.499999999708154341, 35.49999999900384751, -25.50000000000000000 ) ) ;
#1692 = DIRECTION ( 'NONE',  ( 0.000000000000000000, 0.000000000000000000, 1.000000000000000000 ) ) ;
#1693 = EDGE_CURVE ( 'NONE', #10146, #11081, #6719, .T. ) ;
#1694 = VERTEX_POINT ( 'NONE', #16697 ) ;
#1696 = EDGE_LOOP ( 'NONE', ( #4486, #11895, #583, #986, #20627 ) ) ;
#1695 = ORIENTED_EDGE ( 'NONE', *, *, #16541, .T. ) ;
#1697 = ORIENTED_EDGE ( 'NONE', *, *, #2183, .F. ) ;
#1699 = EDGE_LOOP ( 'NONE', ( #6758, #1938, #5310, #2617, #17509 ) ) ;
#1698 = ORIENTED_EDGE ( 'NONE', *, *, #1286, .F. ) ;
#1700 = ORIENTED_EDGE ( 'NONE', *, *, #333, .T. ) ;
#1701 = EDGE_LOOP ( 'NONE', ( #3380, #9857, #18964, #1457 ) ) ;
#1702 = ORIENTED_EDGE ( 'NONE', *, *, #17416, .F. ) ;
#1703 = DIRECTION ( 'NONE',  ( -1.858632295689435609E-16, -1.000000000000000000, 0.000000000000000000 ) ) ;
#1704 = AXIS2_PLACEMENT_3D ( 'NONE', #17732, #23164, #21278 ) ;
#1705 = CIRCLE ( 'NONE', #16346, 2.500000000000009326 ) ;
#1706 = CARTESIAN_POINT ( 'NONE',  ( 0.000000000000000000, 0.000000000000000000, 0.000000000000000000 ) ) ;
#1707 = CARTESIAN_POINT ( 'NONE',  ( 4.175813232069142344, 2.061359961916322980, 3.570380186727409200 ) ) ;
#1708 = CARTESIAN_POINT ( 'NONE',  ( -12.84999999999999964, -6.938893903907228378E-15, 5.749999999999991118 ) ) ;
#1709 = DIRECTION ( 'NONE',  ( 3.330669073875432643E-16, 4.437342591868153746E-31, -1.000000000000000000 ) ) ;
#1710 = PLANE ( 'NONE',  #19487 ) ;
#1711 = CARTESIAN_POINT ( 'NONE',  ( -4.207491450040681258, 2.029819825146493617, -3.671670828759563854 ) ) ;
#1712 = SURFACE_STYLE_USAGE ( .BOTH. , #19589 ) ;
#1713 = CARTESIAN_POINT ( 'NONE',  ( 7.500000000000007105, -5.999999999999981348, 12.24999999999998224 ) ) ;
#1714 = CARTESIAN_POINT ( 'NONE',  ( -50.65685424949262483, -7.200000000000071232, -16.89924331519437928 ) ) ;
#1715 = CARTESIAN_POINT ( 'NONE',  ( -7.500000000000007105, -2.645898033750305522, 9.250000000000035527 ) ) ;
#1716 = ORIENTED_EDGE ( 'NONE', *, *, #12803, .F. ) ;
#1717 = DIRECTION ( 'NONE',  ( 1.000000000000000000, -1.365024226554777796E-62, 2.013525853228508713E-32 ) ) ;
#1718 = CARTESIAN_POINT ( 'NONE',  ( 5.600000000000000533, -2.020725942163764444, 3.499999999999985789 ) ) ;
#1720 = ORIENTED_EDGE ( 'NONE', *, *, #15193, .T. ) ;
#1719 = ORIENTED_EDGE ( 'NONE', *, *, #2803, .T. ) ;
#1721 = ORIENTED_EDGE ( 'NONE', *, *, #4503, .F. ) ;
#1722 = ORIENTED_EDGE ( 'NONE', *, *, #14532, .T. ) ;
#1723 = EDGE_CURVE ( 'NONE', #19565, #9737, #4469, .T. ) ;
#1724 = CARTESIAN_POINT ( 'NONE',  ( 73.50000000000116529, -13.52760560296348302, 3.469446951953614189E-14 ) ) ;
#1725 = DIRECTION ( 'NONE',  ( 4.392831559381931789E-32, 2.168404344970994323E-16, 1.000000000000000000 ) ) ;
#1726 = CARTESIAN_POINT ( 'NONE',  ( -10.49999999999999467, -2.000000000000001776, 5.750000000000005329 ) ) ;
#1727 = FACE_OUTER_BOUND ( 'NONE', #17848, .T. ) ;
#1728 = CYLINDRICAL_SURFACE ( 'NONE', #12093, 0.5000000000000004441 ) ;
#1729 = CARTESIAN_POINT ( 'NONE',  ( -50.65685424949281668, 1.387778780781445676E-14, 7.500000000000034639 ) ) ;
#1730 =( REPRESENTATION_RELATIONSHIP ('NONE','NONE', #19450, #14072 ) REPRESENTATION_RELATIONSHIP_WITH_TRANSFORMATION ( #4698 )SHAPE_REPRESENTATION_RELATIONSHIP( ) );
#1731 = DIRECTION ( 'NONE',  ( 2.168404344970994323E-16, -1.000000000000000000, 1.577721810442023611E-30 ) ) ;
#1732 = FACE_OUTER_BOUND ( 'NONE', #21728, .T. ) ;
#1733 = LINE ( 'NONE', #14216, #14846 ) ;
#1734 = CARTESIAN_POINT ( 'NONE',  ( 37.77870956205628516, 11.00000000000000000, -10.69139372032722335 ) ) ;
#1735 = DIRECTION ( 'NONE',  ( 0.000000000000000000, -1.000000000000000000, 0.000000000000000000 ) ) ;
#1736 = CARTESIAN_POINT ( 'NONE',  ( -90.63385214007844581, 2.700000000000056577, -7.926881151201908615 ) ) ;
#1737 = PLANE ( 'NONE',  #20149 ) ;
#1738 = AXIS2_PLACEMENT_3D ( 'NONE', #18433, #332, #9267 ) ;
#1739 = CYLINDRICAL_SURFACE ( 'NONE', #10098, 0.4999999999999978351 ) ;
#1740 = CARTESIAN_POINT ( 'NONE',  ( 3.061616997868385113E-16, -1.750000000000001554, 2.500000000000000000 ) ) ;
#1741 = EDGE_LOOP ( 'NONE', ( #12035, #6194, #22439, #10055 ) ) ;
#1742 = EDGE_CURVE ( 'NONE', #10482, #16513, #19865, .T. ) ;
#1743 = VERTEX_POINT ( 'NONE', #11295 ) ;
#1744 = EDGE_CURVE ( 'NONE', #14430, #21672, #18257, .T. ) ;
#1745 = DIRECTION ( 'NONE',  ( -1.135604581876758782E-15, 2.131628207280296771E-14, 1.000000000000000000 ) ) ;
#1746 = ORIENTED_EDGE ( 'NONE', *, *, #17889, .F. ) ;
#1747 = AXIS2_PLACEMENT_3D ( 'NONE', #8327, #15376, #7978 ) ;
#1748 = CARTESIAN_POINT ( 'NONE',  ( -3.534277608971974516, -1.672424706883812062, -3.378451613207310356 ) ) ;
#1749 = CARTESIAN_POINT ( 'NONE',  ( 5.100000000000000533, 0.000000000000000000, -3.469446951953614189E-15 ) ) ;
#1750 = CARTESIAN_POINT ( 'NONE',  ( 3.972066048304784491, -3.435565134476505911, -1.180968096049849869 ) ) ;
#1751 = CIRCLE ( 'NONE', #20541, 4.750000000000000888 ) ;
#1752 = CARTESIAN_POINT ( 'NONE',  ( -3.092868566891418549E-14, 2.686816014504519678, 2.346298152288352146 ) ) ;
#1754 = EDGE_LOOP ( 'NONE', ( #12623, #1498, #12008, #18274 ) ) ;
#1753 = ADVANCED_FACE ( 'NONE', ( #18476 ), #20244, .T. ) ;
#1755 = CARTESIAN_POINT ( 'NONE',  ( 0.000000000000000000, 0.000000000000000000, -5.600000000000000533 ) ) ;
#1756 = DIRECTION ( 'NONE',  ( 2.013525853228507892E-32, 6.902532920683810383E-31, -1.000000000000000000 ) ) ;
#1757 = EDGE_CURVE ( 'NONE', #11721, #1694, #2590, .T. ) ;
#1758 = AXIS2_PLACEMENT_3D ( 'NONE', #10952, #18261, #3785 ) ;
#1759 = CARTESIAN_POINT ( 'NONE',  ( 2.775557561562891351E-14, 8.500000000000003553, -6.499999999999950262 ) ) ;
#1760 = CARTESIAN_POINT ( 'NONE',  ( -8.160037397871475306, -13.99120688549555602, 6.662331851011996875 ) ) ;
#1761 = FACE_BOUND ( 'NONE', #21416, .T. ) ;
#1762 = CARTESIAN_POINT ( 'NONE',  ( 8.954763739086869734, -1.499999999999984013, 6.678571428571429713 ) ) ;
#1763 = CARTESIAN_POINT ( 'NONE',  ( -64.00000000000045475, 0.5000000000000490719, -1.999999999999974021 ) ) ;
#1764 = DIRECTION ( 'NONE',  ( 1.000000000000000000, -4.190823558986610327E-31, 1.733449886265890494E-32 ) ) ;
#1765 = CARTESIAN_POINT ( 'NONE',  ( -4.499999999708154341, 35.99999999900384751, -22.50000000000000000 ) ) ;
#1766 = CARTESIAN_POINT ( 'NONE',  ( -65.00000000000044054, -2.700000000000084110, 2.999999999999947153 ) ) ;
#1767 = ADVANCED_FACE ( 'NONE', ( #5897 ), #490, .T. ) ;
#1768 = ORIENTED_EDGE ( 'NONE', *, *, #752, .T. ) ;
#1769 = VECTOR ( 'NONE', #973, 1000.000000000000000 ) ;
#1770 = EDGE_CURVE ( 'NONE', #7684, #10125, #13996, .T. ) ;
#1771 = EDGE_CURVE ( 'NONE', #22415, #2139, #22955, .T. ) ;
#1772 =( GEOMETRIC_REPRESENTATION_CONTEXT ( 3 ) GLOBAL_UNCERTAINTY_ASSIGNED_CONTEXT ( ( #4602 ) ) GLOBAL_UNIT_ASSIGNED_CONTEXT ( ( #19888, #7082, #5068 ) ) REPRESENTATION_CONTEXT ( 'NONE', 'WORKASPACE' ) );
#1773 = DIRECTION ( 'NONE',  ( -0.5620337693514488864, -0.7884522727909154538, 0.2499220991417978321 ) ) ;
#1775 = VERTEX_POINT ( 'NONE', #12217 ) ;
#1774 = VERTEX_POINT ( 'NONE', #13656 ) ;
#1776 = AXIS2_PLACEMENT_3D ( 'NONE', #8921, #13973, #7050 ) ;
#1778 = ORIENTED_EDGE ( 'NONE', *, *, #3061, .F. ) ;
#1777 = ORIENTED_EDGE ( 'NONE', *, *, #22734, .T. ) ;
#1779 = EDGE_CURVE ( 'NONE', #21726, #16673, #7567, .T. ) ;
#1780 = CARTESIAN_POINT ( 'NONE',  ( -6.962001439796708269, 35.99999999900384751, -26.47597002942762145 ) ) ;
#1781 = DIRECTION ( 'NONE',  ( -3.469446951953634699E-15, 1.000000000000000000, -4.336808689942038246E-15 ) ) ;
#1782 = CARTESIAN_POINT ( 'NONE',  ( 29.00000000029184832, 16.99999999900385461, -18.50000000000000355 ) ) ;
#1783 = EDGE_CURVE ( 'NONE', #11087, #21212, #20847, .T. ) ;
#1784 = CARTESIAN_POINT ( 'NONE',  ( -7.268749084027625429, -11.74104661578623521, 7.689023314178108137 ) ) ;
#1785 = AXIS2_PLACEMENT_3D ( 'NONE', #21770, #12462, #242 ) ;
#1786 = CARTESIAN_POINT ( 'NONE',  ( 3.999999999999989786, -2.309401076758549998, -0.3572655899081733644 ) ) ;
#1787 = EDGE_CURVE ( 'NONE', #9785, #9160, #6352, .T. ) ;
#1788 = CARTESIAN_POINT ( 'NONE',  ( 8.718376657154827569, -13.50000000000004086, 6.820622386032026974 ) ) ;
#1789 = AXIS2_PLACEMENT_3D ( 'NONE', #3022, #2791, #22555 ) ;
#1790 = CARTESIAN_POINT ( 'NONE',  ( -55.05572809000126711, 0.5000000000000143219, -7.500000000000034639 ) ) ;
#1791 = DIRECTION ( 'NONE',  ( 2.172745813409349776E-17, -1.000000000000000000, 1.309377075419428048E-16 ) ) ;
#1792 = DIRECTION ( 'NONE',  ( -2.013525853228507892E-32, -6.902532920683810383E-31, 1.000000000000000000 ) ) ;
#1793 = CARTESIAN_POINT ( 'NONE',  ( 4.211140560182139225, 2.431303136016540911, -3.745885042887430405 ) ) ;
#1794 = AXIS2_PLACEMENT_3D ( 'NONE', #17282, #15404, #6475 ) ;
#1795 = DIRECTION ( 'NONE',  ( 0.000000000000000000, 0.000000000000000000, 1.000000000000000000 ) ) ;
#1796 = CARTESIAN_POINT ( 'NONE',  ( 4.229990831856818900, 1.750000000000002442, 2.173440963673456405 ) ) ;
#1797 = AXIS2_PLACEMENT_3D ( 'NONE', #12494, #3572, #12734 ) ;
#1798 = DIRECTION ( 'NONE',  ( -0.7313537016191746787, -0.6819983600624940356, -1.072890437865584285E-16 ) ) ;
#1799 = DIRECTION ( 'NONE',  ( 3.885780586188016830E-16, 4.437342591868156373E-31, -1.000000000000000000 ) ) ;
#1800 = CARTESIAN_POINT ( 'NONE',  ( 8.725359747074517003, -0.4999999928004930649, 6.816426071237541073 ) ) ;
#1801 = ORIENTED_EDGE ( 'NONE', *, *, #3375, .T. ) ;
#1803 = ORIENTED_EDGE ( 'NONE', *, *, #18662, .T. ) ;
#1802 = ORIENTED_EDGE ( 'NONE', *, *, #17536, .F. ) ;
#1804 = AXIS2_PLACEMENT_3D ( 'NONE', #15904, #4974, #22755 ) ;
#1805 = ORIENTED_EDGE ( 'NONE', *, *, #4040, .F. ) ;
#1807 = ORIENTED_EDGE ( 'NONE', *, *, #17435, .T. ) ;
#1806 = ORIENTED_EDGE ( 'NONE', *, *, #14276, .F. ) ;
#1808 = CIRCLE ( 'NONE', #10459, 2.054999999999999716 ) ;
#1809 = ORIENTED_EDGE ( 'NONE', *, *, #8067, .T. ) ;
#1810 = EDGE_CURVE ( 'NONE', #5384, #15489, #6597, .T. ) ;
#1811 = ORIENTED_EDGE ( 'NONE', *, *, #2933, .F. ) ;
#1812 = ORIENTED_EDGE ( 'NONE', *, *, #16958, .F. ) ;
#1813 = CARTESIAN_POINT ( 'NONE',  ( 0.000000000000000000, 0.000000000000000000, 3.499999999999975131 ) ) ;
#1814 = AXIS2_PLACEMENT_3D ( 'NONE', #21549, #12588, #18016 ) ;
#1815 = VECTOR ( 'NONE', #2710, 1000.000000000000227 ) ;
#1816 = DIRECTION ( 'NONE',  ( 0.7071067811865718866, 0.7071067811865232589, 0.000000000000000000 ) ) ;
#1817 = CARTESIAN_POINT ( 'NONE',  ( -2.000000000000015543, 3.464101615137746837, 0.000000000000000000 ) ) ;
#1818 = EDGE_CURVE ( 'NONE', #7626, #21952, #22831, .T. ) ;
#1819 = DIRECTION ( 'NONE',  ( 1.000000000000000000, 3.254448077276381206E-32, 1.066788928082016908E-26 ) ) ;
#1820 = DIRECTION ( 'NONE',  ( 0.000000000000000000, 0.000000000000000000, 1.000000000000000000 ) ) ;
#1821 = LINE ( 'NONE', #23253, #8978 ) ;
#1822 = CARTESIAN_POINT ( 'NONE',  ( 73.50000000000116529, -6.999999999999811706, -2.549999999999999822 ) ) ;
#1823 = CARTESIAN_POINT ( 'NONE',  ( 2.775557561562891351E-14, 11.00000000000000000, -12.50000000000001066 ) ) ;
#1824 = CARTESIAN_POINT ( 'NONE',  ( -4.365918574175959854, 13.48846683486500808, -16.01652206364978781 ) ) ;
#1825 = AXIS2_PLACEMENT_3D ( 'NONE', #606, #12956, #7769 ) ;
#1826 = CARTESIAN_POINT ( 'NONE',  ( -8.715898959466867879, -1.502431622389268417, 6.833978265953976283 ) ) ;
#1827 = ORIENTED_EDGE ( 'NONE', *, *, #20596, .F. ) ;
#1828 = CIRCLE ( 'NONE', #22491, 0.5000000000000038858 ) ;
#1829 = DIRECTION ( 'NONE',  ( 3.885780586188016830E-16, 4.437342591868156373E-31, -1.000000000000000000 ) ) ;
#1830 = CARTESIAN_POINT ( 'NONE',  ( -57.28378781035996070, -2.700000000000049472, 8.541666666666781538 ) ) ;
#1832 = ORIENTED_EDGE ( 'NONE', *, *, #4323, .F. ) ;
#1831 = ORIENTED_EDGE ( 'NONE', *, *, #764, .T. ) ;
#1833 = ORIENTED_EDGE ( 'NONE', *, *, #348, .F. ) ;
#1834 = VERTEX_POINT ( 'NONE', #19062 ) ;
#1835 =( GEOMETRIC_REPRESENTATION_CONTEXT ( 3 ) GLOBAL_UNCERTAINTY_ASSIGNED_CONTEXT ( ( #19192 ) ) GLOBAL_UNIT_ASSIGNED_CONTEXT ( ( #12532, #5487, #10539 ) ) REPRESENTATION_CONTEXT ( 'NONE', 'WORKASPACE' ) );
#1836 = CARTESIAN_POINT ( 'NONE',  ( 42.50000000000014921, 5.500000000000001776, 2.000000000000071054 ) ) ;
#1837 = CARTESIAN_POINT ( 'NONE',  ( 1.849731447993483435, 1.560358803165483366, 4.749999999999998224 ) ) ;
#1838 = CARTESIAN_POINT ( 'NONE',  ( 2.298974087845762959, -1.453757124411863222, 4.749999999999999112 ) ) ;
#1839 = CYLINDRICAL_SURFACE ( 'NONE', #20758, 4.000000000000045297 ) ;
#1840 = VECTOR ( 'NONE', #12414, 1000.000000000000000 ) ;
#1841 = DIRECTION ( 'NONE',  ( -2.220446049250313081E-16, 1.000000000000000000, -7.025792437124636392E-31 ) ) ;
#1842 = DIRECTION ( 'NONE',  ( 0.000000000000000000, -0.000000000000000000, -1.000000000000000000 ) ) ;
#1843 = CARTESIAN_POINT ( 'NONE',  ( 8.832214555408096857, -12.50000000000003375, 6.752214322824835691 ) ) ;
#1844 = DIRECTION ( 'NONE',  ( 0.000000000000000000, -1.000000000000000000, 0.000000000000000000 ) ) ;
#1845 = LINE ( 'NONE', #5152, #3945 ) ;
#1846 = CARTESIAN_POINT ( 'NONE',  ( 10.50000000000000888, -1.500000000000001332, 5.750000000000005329 ) ) ;
#1847 = AXIS2_PLACEMENT_3D ( 'NONE', #21299, #15754, #15635 ) ;
#1848 = CARTESIAN_POINT ( 'NONE',  ( -47.82842712474641189, -4.371572875253862733, 7.500000000000047962 ) ) ;
#1849 = CARTESIAN_POINT ( 'NONE',  ( -4.000000000000003553, -2.309401076758525573, -5.600000000000000533 ) ) ;
#1850 = CARTESIAN_POINT ( 'NONE',  ( -4.141042297810708206, 2.227970268150420541, -3.687027686973645135 ) ) ;
#1851 = PRESENTATION_LAYER_ASSIGNMENT (  '', '', ( #16115 ) ) ;
#1852 = EDGE_CURVE ( 'NONE', #3527, #7794, #275, .T. ) ;
#1853 = FACE_OUTER_BOUND ( 'NONE', #7005, .T. ) ;
#1854 = CARTESIAN_POINT ( 'NONE',  ( -5.551115123125782702E-14, 4.618802153517065356, -0.5000000000000004441 ) ) ;
#1855 = ORIENTED_EDGE ( 'NONE', *, *, #16854, .T. ) ;
#1856 = SHAPE_REPRESENTATION ( 'Link', ( #22115 ), #3350 ) ;
#1857 = ORIENTED_EDGE ( 'NONE', *, *, #6505, .F. ) ;
#1858 = CARTESIAN_POINT ( 'NONE',  ( -6.226186441994419063, 36.09747688189035131, -28.02588720118439269 ) ) ;
#1859 = ORIENTED_EDGE ( 'NONE', *, *, #20481, .T. ) ;
#1860 = AXIS2_PLACEMENT_3D ( 'NONE', #19707, #7012, #12163 ) ;
#1861 = CARTESIAN_POINT ( 'NONE',  ( -3.191035955565411975, 1.584759246591057824, -3.972963596181423362 ) ) ;
#1862 = LINE ( 'NONE', #9046, #20910 ) ;
#1863 = CARTESIAN_POINT ( 'NONE',  ( 4.033901012035399525, -2.321269032828001233, -2.979444097106729750 ) ) ;
#1864 = CARTESIAN_POINT ( 'NONE',  ( 2.100000000000000089, -2.611376934403532807E-15, -4.694516984716119445 ) ) ;
#1865 = ORIENTED_EDGE ( 'NONE', *, *, #2806, .F. ) ;
#1866 = CARTESIAN_POINT ( 'NONE',  ( -6.000000000000074607, 1.999999999999960032, 7.500000000000062172 ) ) ;
#1867 = CARTESIAN_POINT ( 'NONE',  ( 1.200000000000006617, 0.6000000000000067502, -4.543283425070335113 ) ) ;
#1868 = CARTESIAN_POINT ( 'NONE',  ( -43.10883117545713361, 4.565685424949256443, 8.000000000000035527 ) ) ;
#1869 = DIRECTION ( 'NONE',  ( 1.000000000000000000, -1.389842848855773583E-62, 2.013525853228507892E-32 ) ) ;
#1870 = CARTESIAN_POINT ( 'NONE',  ( 5.599999999999991651, 6.539831464966449098E-16, -5.200000000000001066 ) ) ;
#1871 = DIRECTION ( 'NONE',  ( 1.000000000000000000, 2.699383410053119644E-30, 3.330669073875432643E-16 ) ) ;
#1872 = CARTESIAN_POINT ( 'NONE',  ( 4.158413352280815545, 2.044871626972852408, -3.541821552872977286 ) ) ;
#1873 = CARTESIAN_POINT ( 'NONE',  ( 3.878096787214420083, -2.680238624820968418, 2.357690525401573645 ) ) ;
#1874 = DIRECTION ( 'NONE',  ( 0.000000000000000000, 0.000000000000000000, -1.000000000000000000 ) ) ;
#1875 = EDGE_CURVE ( 'NONE', #5138, #4916, #11230, .T. ) ;
#1876 = DIRECTION ( 'NONE',  ( 0.000000000000000000, 0.000000000000000000, 1.000000000000000000 ) ) ;
#1877 = ORIENTED_EDGE ( 'NONE', *, *, #8108, .T. ) ;
#1878 = EDGE_CURVE ( 'NONE', #226, #5138, #15683, .T. ) ;
#1879 = EDGE_CURVE ( 'NONE', #7941, #3485, #4038, .T. ) ;
#1881 = ORIENTED_EDGE ( 'NONE', *, *, #6149, .T. ) ;
#1880 = VERTEX_POINT ( 'NONE', #10126 ) ;
#1882 = EDGE_CURVE ( 'NONE', #11578, #13234, #10444, .T. ) ;
#1883 = VERTEX_POINT ( 'NONE', #6713 ) ;
#1885 = ORIENTED_EDGE ( 'NONE', *, *, #15397, .T. ) ;
#1884 = ORIENTED_EDGE ( 'NONE', *, *, #13567, .T. ) ;
#1886 = CARTESIAN_POINT ( 'NONE',  ( 0.6810597143191978731, 4.461075778259148805, -3.598441714920549206 ) ) ;
#1887 = DIRECTION ( 'NONE',  ( 0.000000000000000000, -1.000000000000000000, 0.000000000000000000 ) ) ;
#1888 = CARTESIAN_POINT ( 'NONE',  ( 7.972478112619588941, -12.36350260656811528, 7.628219499134369919 ) ) ;
#1889 = VECTOR ( 'NONE', #3441, 1000.000000000000000 ) ;
#1890 = DIRECTION ( 'NONE',  ( -1.000000000000000000, 4.190823558986610327E-31, -1.733449886265890494E-32 ) ) ;
#1891 = CARTESIAN_POINT ( 'NONE',  ( 0.4500000002918510544, 42.99999999900385461, -15.99999999999999289 ) ) ;
#1892 = EDGE_CURVE ( 'NONE', #4169, #16118, #8245, .T. ) ;
#1893 =( BOUNDED_SURFACE ( )  B_SPLINE_SURFACE ( 3, 2, ( 
 ( #2460, #11282, #7534 ),
 ( #18354, #18464, #20243 ),
 ( #9296, #5774, #6118 ),
 ( #18586, #9418, #16915 ),
 ( #16455, #13176, #4330 ),
 ( #592, #367, #7757 ) ),
 .UNSPECIFIED., .F., .F., .T. ) 
 B_SPLINE_SURFACE_WITH_KNOTS ( ( 4, 2, 4 ),
 ( 3, 3 ),
 ( 0.01651999345535505245, 0.01858032176739834312, 0.02064065007944163727 ),
 ( 0.000000000000000000, 1.000000000000000000 ),
 .UNSPECIFIED. ) 
 GEOMETRIC_REPRESENTATION_ITEM ( )  RATIONAL_B_SPLINE_SURFACE ( (
 ( 1.000000000000000000, 0.8047781103519393575, 1.000000000000000000),
 ( 1.000000000000000000, 0.8123785825603665467, 1.000000000000000000),
 ( 1.000000000000000000, 0.8190671539789206035, 1.000000000000000000),
 ( 1.000000000000000000, 0.8192352254833937808, 1.000000000000000000),
 ( 1.000000000000000000, 0.8126129677212307056, 1.000000000000000000),
 ( 1.000000000000000000, 0.8047712537969730073, 1.000000000000000000) ) ) 
 REPRESENTATION_ITEM ( '' )  SURFACE ( )  );
#1894 = FACE_OUTER_BOUND ( 'NONE', #9998, .T. ) ;
#1896 = ADVANCED_FACE ( 'NONE', ( #22591 ), #19404, .T. ) ;
#1895 = FACE_OUTER_BOUND ( 'NONE', #18949, .T. ) ;
#1897 = DIRECTION ( 'NONE',  ( -1.000000000000000000, 4.615739097524200579E-16, 1.134196829589820086E-15 ) ) ;
#1898 = CARTESIAN_POINT ( 'NONE',  ( 0.000000000000000000, 0.000000000000000000, -4.974599999999998801 ) ) ;
#1899 = DIRECTION ( 'NONE',  ( 0.000000000000000000, -1.000000000000000000, 0.000000000000000000 ) ) ;
#1900 = CARTESIAN_POINT ( 'NONE',  ( 5.261076337303422612, -1.454929939081816226, -0.3875484812921113353 ) ) ;
#1901 = CARTESIAN_POINT ( 'NONE',  ( -6.938893903907228378E-14, -4.618802153517020059, -5.242734410091827613 ) ) ;
#1902 = FACE_OUTER_BOUND ( 'NONE', #22361, .T. ) ;
#1903 = CARTESIAN_POINT ( 'NONE',  ( 3.999999999999935163, -1.942223658245677775, -0.3516579909967328943 ) ) ;
#1904 = EDGE_CURVE ( 'NONE', #16829, #13948, #12688, .T. ) ;
#1905 = DIRECTION ( 'NONE',  ( -0.7071067811865485719, 0.7071067811865464625, 1.010793663541191362E-16 ) ) ;
#1906 = ORIENTED_EDGE ( 'NONE', *, *, #10371, .F. ) ;
#1907 = EDGE_CURVE ( 'NONE', #14019, #15168, #4796, .T. ) ;
#1908 = AXIS2_PLACEMENT_3D ( 'NONE', #16553, #16096, #10814 ) ;
#1909 = AXIS2_PLACEMENT_3D ( 'NONE', #12173, #5123, #19476 ) ;
#1911 = ORIENTED_EDGE ( 'NONE', *, *, #17784, .T. ) ;
#1910 = VERTEX_POINT ( 'NONE', #1191 ) ;
#1912 = EDGE_CURVE ( 'NONE', #22610, #5349, #17519, .T. ) ;
#1913 = EDGE_LOOP ( 'NONE', ( #8994, #14076, #21538, #22655 ) ) ;
#1915 = ORIENTED_EDGE ( 'NONE', *, *, #4798, .F. ) ;
#1914 = ORIENTED_EDGE ( 'NONE', *, *, #5831, .T. ) ;
#1916 = EDGE_LOOP ( 'NONE', ( #16349, #12628 ) ) ;
#1917 = CARTESIAN_POINT ( 'NONE',  ( 4.093692494532772841, 2.021783646005771207, 3.501831996793840052 ) ) ;
#1918 = ORIENTED_EDGE ( 'NONE', *, *, #12888, .F. ) ;
#1919 = VERTEX_POINT ( 'NONE', #6956 ) ;
#1920 = DIRECTION ( 'NONE',  ( 1.000000000000000000, 2.699383410053119644E-30, 3.330669073875432643E-16 ) ) ;
#1921 =( NAMED_UNIT ( * ) SI_UNIT ( $, .STERADIAN. ) SOLID_ANGLE_UNIT ( ) );
#1922 = DIRECTION ( 'NONE',  ( -1.333893503340774882E-15, -2.778352770573747380E-17, -1.000000000000000000 ) ) ;
#1923 = FACE_OUTER_BOUND ( 'NONE', #21813, .T. ) ;
#1924 = DIRECTION ( 'NONE',  ( -1.000000000000000000, -2.172745813409349776E-17, 2.775557561562883647E-17 ) ) ;
#1925 = DIRECTION ( 'NONE',  ( 2.220446049250313081E-16, -1.000000000000000000, 7.025792437124636392E-31 ) ) ;
#1926 = CIRCLE ( 'NONE', #17697, 3.000000000000011546 ) ;
#1927 = AXIS2_PLACEMENT_3D ( 'NONE', #3972, #342, #7738 ) ;
#1928 = DIRECTION ( 'NONE',  ( -1.000000000000000000, -2.699383410053119644E-30, -3.330669073875432643E-16 ) ) ;
#1929 = CARTESIAN_POINT ( 'NONE',  ( 54.42435809754115894, 0.4999999999999449329, -5.999999999999950262 ) ) ;
#1930 = CARTESIAN_POINT ( 'NONE',  ( 0.1217565302851083830, -2.351289329882206403, -2.927447417349482883 ) ) ;
#1931 = CARTESIAN_POINT ( 'NONE',  ( 12.84999999999997300, -14.00000000000005329, 2.550000000000052669 ) ) ;
#1932 = EDGE_CURVE ( 'NONE', #20684, #7007, #22440, .T. ) ;
#1933 = CARTESIAN_POINT ( 'NONE',  ( 5.550000000291854363, 42.99999999900385461, -25.50000000000000355 ) ) ;
#1934 = ORIENTED_EDGE ( 'NONE', *, *, #20891, .F. ) ;
#1935 = SHAPE_REPRESENTATION_RELATIONSHIP ( 'NONE' , 'NONE' ,  #981, #5834 ) ;
#1936 = FACE_OUTER_BOUND ( 'NONE', #20385, .T. ) ;
#1938 = ORIENTED_EDGE ( 'NONE', *, *, #3195, .T. ) ;
#1937 = ORIENTED_EDGE ( 'NONE', *, *, #9948, .T. ) ;
#1939 = ORIENTED_EDGE ( 'NONE', *, *, #20832, .F. ) ;
#1940 = B_SPLINE_CURVE_WITH_KNOTS ( 'NONE', 3,
 ( #6145, #13319, #14419, #20501 ),
 .UNSPECIFIED., .F., .F.,
 ( 4, 4 ),
 ( 0.01162760039383341909, 0.01599369037747973635 ),
 .UNSPECIFIED. ) ;
#1941 = AXIS2_PLACEMENT_3D ( 'NONE', #11300, #14717, #8769 ) ;
#1942 = AXIS2_PLACEMENT_3D ( 'NONE', #17252, #1165, #19145 ) ;
#1943 = EDGE_LOOP ( 'NONE', ( #17781, #12744, #2271, #11404 ) ) ;
#1944 = ORIENTED_EDGE ( 'NONE', *, *, #21206, .T. ) ;
#1945 = EDGE_LOOP ( 'NONE', ( #11982, #5081, #22904, #18569 ) ) ;
#1946 = FACE_OUTER_BOUND ( 'NONE', #3552, .T. ) ;
#1947 = CARTESIAN_POINT ( 'NONE',  ( 108.2426266706970353, -6.527605602963587828, 6.500000000000199840 ) ) ;
#1948 = CARTESIAN_POINT ( 'NONE',  ( 2.500000000000002220, 0.000000000000000000, -25.03750572909317285 ) ) ;
#1949 = DIRECTION ( 'NONE',  ( 3.885780586188016830E-16, 4.437342591868156373E-31, -1.000000000000000000 ) ) ;
#1950 = CIRCLE ( 'NONE', #6480, 6.500000000000075495 ) ;
#1951 = PLANE ( 'NONE',  #19958 ) ;
#1952 = FACE_BOUND ( 'NONE', #15450, .T. ) ;
#1953 = CARTESIAN_POINT ( 'NONE',  ( -1.316424159404522588E-14, -24.99999999999998224, 4.750000000000013323 ) ) ;
#1954 = CARTESIAN_POINT ( 'NONE',  ( 2.918498775983380256E-10, -9.961476088449217059E-10, -19.00000000000000355 ) ) ;
#1955 = CIRCLE ( 'NONE', #8719, 6.500000000000075495 ) ;
#1956 = CARTESIAN_POINT ( 'NONE',  ( 88.75737332930596324, -13.52760560296348302, -6.499999999999964473 ) ) ;
#1957 = DIRECTION ( 'NONE',  ( -1.000000000000000000, -3.254448077276381206E-32, -1.066788928082016908E-26 ) ) ;
#1958 = VECTOR ( 'NONE', #17366, 1000.000000000000000 ) ;
#1959 = EDGE_CURVE ( 'NONE', #15940, #5921, #19878, .T. ) ;
#1960 = CARTESIAN_POINT ( 'NONE',  ( 37.45482484129320966, 0.2122202663360098496, -10.04362427881557274 ) ) ;
#1961 = TOROIDAL_SURFACE ( 'NONE', #15481, 3.500000000000000000, 0.5000000000000000000 ) ;
#1962 = VECTOR ( 'NONE', #19867, 1000.000000000000114 ) ;
#1963 = CYLINDRICAL_SURFACE ( 'NONE', #11964, 0.5000000000000004441 ) ;
#1964 = FACE_OUTER_BOUND ( 'NONE', #13440, .T. ) ;
#1965 = EDGE_LOOP ( 'NONE', ( #1982, #10746, #15822, #4725 ) ) ;
#1966 = EDGE_CURVE ( 'NONE', #3408, #6309, #5169, .T. ) ;
#1967 = CIRCLE ( 'NONE', #15113, 0.5000000000000038858 ) ;
#1968 = ORIENTED_EDGE ( 'NONE', *, *, #20201, .F. ) ;
#1969 = B_SPLINE_CURVE_WITH_KNOTS ( 'NONE', 3,
 ( #22394, #11321, #5930, #4147, #9577, #16954 ),
 .UNSPECIFIED., .F., .F.,
 ( 4, 2, 4 ),
 ( 0.002044882221487500686, 0.003063384235218499785, 0.004081886248949498017 ),
 .UNSPECIFIED. ) ;
#1970 = DIRECTION ( 'NONE',  ( 1.550910762415566494E-16, 1.000000000000000000, -8.135128085091684243E-31 ) ) ;
#1971 = FACE_OUTER_BOUND ( 'NONE', #6649, .T. ) ;
#1972 = ORIENTED_EDGE ( 'NONE', *, *, #18954, .F. ) ;
#1973 = VECTOR ( 'NONE', #19204, 1000.000000000000000 ) ;
#1974 = CARTESIAN_POINT ( 'NONE',  ( -6.959810536856695151, 36.00015702695179698, -18.51059057611807646 ) ) ;
#1975 = AXIS2_PLACEMENT_3D ( 'NONE', #8643, #15800, #4991 ) ;
#1976 = AXIS2_PLACEMENT_3D ( 'NONE', #10040, #22166, #20755 ) ;
#1977 = CARTESIAN_POINT ( 'NONE',  ( 0.3126073911695753660, -2.020725942163792421, -3.499999999999996891 ) ) ;
#1978 = CARTESIAN_POINT ( 'NONE',  ( 8.565230440156009095, -12.00000000000005151, 6.320505311736963172 ) ) ;
#1979 = EDGE_CURVE ( 'NONE', #8147, #2421, #17962, .T. ) ;
#1980 = AXIS2_PLACEMENT_3D ( 'NONE', #4434, #15487, #15248 ) ;
#1981 = SURFACE_STYLE_FILL_AREA ( #19761 ) ;
#1982 = ORIENTED_EDGE ( 'NONE', *, *, #448, .F. ) ;
#1983 = CARTESIAN_POINT ( 'NONE',  ( 119.5756419024615553, -11.00000000000006573, 6.500000000000012434 ) ) ;
#1984 = CARTESIAN_POINT ( 'NONE',  ( 3.951447005078449148, -3.704664227300103807, -0.5833333333333333703 ) ) ;
#1985 = LINE ( 'NONE', #7524, #10565 ) ;
#1986 = CARTESIAN_POINT ( 'NONE',  ( 7.735962016526152674, -13.93008758169059469, 7.174192622767042948 ) ) ;
#1987 = CARTESIAN_POINT ( 'NONE',  ( 7.176407415342080043, -13.63581929081302668, 8.314790908397570846 ) ) ;
#1988 = CARTESIAN_POINT ( 'NONE',  ( 4.024499207728656991, -2.323545700935616853, -3.572172305156546823 ) ) ;
#1989 = DIRECTION ( 'NONE',  ( 0.000000000000000000, 0.000000000000000000, 1.000000000000000000 ) ) ;
#1990 = SURFACE_SIDE_STYLE ('',( #8950 ) ) ;
#1991 = AXIS2_PLACEMENT_3D ( 'NONE', #16077, #10680, #21636 ) ;
#1992 = DIRECTION ( 'NONE',  ( -1.000000000000000000, -2.699383410053119644E-30, -3.330669073875432643E-16 ) ) ;
#1993 = CIRCLE ( 'NONE', #20796, 0.5000000000000004441 ) ;
#1994 = AXIS2_PLACEMENT_3D ( 'NONE', #1866, #1650, #5061 ) ;
#1995 = AXIS2_PLACEMENT_3D ( 'NONE', #21572, #10948, #10730 ) ;
#1996 = AXIS2_PLACEMENT_3D ( 'NONE', #15198, #4731, #13791 ) ;
#1997 = APPLICATION_PROTOCOL_DEFINITION ( 'draft international standard', 'automotive_design', 1998, #22003 ) ;
#1999 = VERTEX_POINT ( 'NONE', #19644 ) ;
#1998 = ORIENTED_EDGE ( 'NONE', *, *, #5798, .T. ) ;
#2000 = ORIENTED_EDGE ( 'NONE', *, *, #370, .T. ) ;
#2001 = PRODUCT_DEFINITION ( 'UNKNOWN', '', #1132, #10993 ) ;
#2003 = ORIENTED_EDGE ( 'NONE', *, *, #17889, .T. ) ;
#2002 = ORIENTED_EDGE ( 'NONE', *, *, #11745, .T. ) ;
#2004 = DIRECTION ( 'NONE',  ( -1.000000000000000000, 1.773272886554051558E-14, -3.854941057726199147E-16 ) ) ;
#2005 = DIRECTION ( 'NONE',  ( -0.7071067811865485719, 0.7071067811865464625, 1.010793663541191485E-16 ) ) ;
#2006 = EDGE_CURVE ( 'NONE', #13205, #15190, #3678, .T. ) ;
#2007 = CARTESIAN_POINT ( 'NONE',  ( 8.165409815605739752, -11.99182595524110084, 6.581206704444357847 ) ) ;
#2008 = AXIS2_PLACEMENT_3D ( 'NONE', #4771, #3017, #6657 ) ;
#2009 = CIRCLE ( 'NONE', #18541, 3.933012701892234730 ) ;
#2010 = CARTESIAN_POINT ( 'NONE',  ( -6.999999999999976907, -11.18103031733298280, 8.693499985977949152 ) ) ;
#2011 = CIRCLE ( 'NONE', #9164, 2.550000000000002043 ) ;
#2012 = DIRECTION ( 'NONE',  ( 0.000000000000000000, 0.000000000000000000, -1.000000000000000000 ) ) ;
#2013 = LINE ( 'NONE', #7550, #15143 ) ;
#2014 = AXIS2_PLACEMENT_3D ( 'NONE', #21294, #11269, #13039 ) ;
#2015 = DIRECTION ( 'NONE',  ( -1.000000000000000000, 1.847414967615758933E-47, -3.885780586188017323E-16 ) ) ;
#2016 = CARTESIAN_POINT ( 'NONE',  ( 2.775557561562891351E-14, 10.49999999999999822, -9.999999999999968026 ) ) ;
#2017 = EDGE_CURVE ( 'NONE', #2950, #9648, #22454, .T. ) ;
#2018 = DIRECTION ( 'NONE',  ( 0.7071067811865485719, -0.7071067811865463515, -1.010793663541191485E-16 ) ) ;
#2019 = DIRECTION ( 'NONE',  ( 0.7071067811865464625, 0.7071067811865486830, 2.121016688166348642E-16 ) ) ;
#2020 = CARTESIAN_POINT ( 'NONE',  ( 42.50000000000020606, 2.499999999999998668, -13.00000000000002487 ) ) ;
#2021 = DIRECTION ( 'NONE',  ( -1.000000000000000000, 0.000000000000000000, 0.000000000000000000 ) ) ;
#2022 = ADVANCED_FACE ( 'NONE', ( #16 ), #14344, .T. ) ;
#2023 = CARTESIAN_POINT ( 'NONE',  ( 3.972709601346594344, -2.746729940827189687, 2.374099244652733365 ) ) ;
#2024 = CARTESIAN_POINT ( 'NONE',  ( -2.100000000000000089, 3.008176102356893744E-15, -0.2800830152838794107 ) ) ;
#2025 = CARTESIAN_POINT ( 'NONE',  ( -5.416517661024267127, 35.99999999900385461, -19.34908248715211698 ) ) ;
#2026 = CARTESIAN_POINT ( 'NONE',  ( 8.721922330811608504, -0.01237189218583836445, 6.818491697976307719 ) ) ;
#2027 = ORIENTED_EDGE ( 'NONE', *, *, #23005, .T. ) ;
#2028 = CIRCLE ( 'NONE', #11046, 2.550000000000010481 ) ;
#2029 = CONICAL_SURFACE ( 'NONE', #11049, 4.000000000000000000, 1.047197551196595855 ) ;
#2031 = ORIENTED_EDGE ( 'NONE', *, *, #6558, .T. ) ;
#2030 = ORIENTED_EDGE ( 'NONE', *, *, #21313, .F. ) ;
#2032 = AXIS2_PLACEMENT_3D ( 'NONE', #3124, #22998, #6884 ) ;
#2033 = EDGE_LOOP ( 'NONE', ( #15017, #2998, #18334, #5348 ) ) ;
#2034 = EDGE_CURVE ( 'NONE', #10886, #5077, #2545, .T. ) ;
#2036 = EDGE_LOOP ( 'NONE', ( #4334, #5262, #8876, #17329 ) ) ;
#2035 = ORIENTED_EDGE ( 'NONE', *, *, #21054, .T. ) ;
#2037 = ORIENTED_EDGE ( 'NONE', *, *, #20019, .F. ) ;
#2038 = CARTESIAN_POINT ( 'NONE',  ( 12.84999999999995879, -12.50000000000011191, -5.749999999999907629 ) ) ;
#2039 = EDGE_LOOP ( 'NONE', ( #11308, #14115, #3123 ) ) ;
#2040 = EDGE_CURVE ( 'NONE', #10112, #11689, #17882, .T. ) ;
#2041 = ORIENTED_EDGE ( 'NONE', *, *, #13149, .F. ) ;
#2042 = DIRECTION ( 'NONE',  ( -1.000000000000000000, -2.699383410053119644E-30, -3.330669073875432643E-16 ) ) ;
#2043 = SURFACE_STYLE_USAGE ( .BOTH. , #21820 ) ;
#2044 = LINE ( 'NONE', #9111, #6756 ) ;
#2045 = DIRECTION ( 'NONE',  ( -1.000000000000000000, 4.437342591868175641E-31, -3.330669073875457788E-16 ) ) ;
#2046 = CIRCLE ( 'NONE', #8063, 2.100000000000011635 ) ;
#2047 = EDGE_CURVE ( 'NONE', #12739, #15071, #304, .T. ) ;
#2048 = CARTESIAN_POINT ( 'NONE',  ( 4.158413352280808439, -2.044871626972824430, -3.541821552872959966 ) ) ;
#2049 = LINE ( 'NONE', #18181, #15713 ) ;
#2050 = EDGE_CURVE ( 'NONE', #18266, #6638, #12897, .T. ) ;
#2051 = DIRECTION ( 'NONE',  ( 1.000000000000000000, 2.168404344971017743E-16, -1.780660105995169760E-30 ) ) ;
#2052 = DIRECTION ( 'NONE',  ( -0.000000000000000000, -0.000000000000000000, 1.000000000000000000 ) ) ;
#2053 = DIRECTION ( 'NONE',  ( -0.9878135252003127365, -2.193386639427060722E-16, 0.1556420233463029767 ) ) ;
#2054 = FACE_OUTER_BOUND ( 'NONE', #6213, .T. ) ;
#2055 = EDGE_LOOP ( 'NONE', ( #1464, #14627, #10245, #18618 ) ) ;
#2056 = PRODUCT_DEFINITION_CONTEXT ( 'detailed design', #17494, 'design' ) ;
#2057 = CYLINDRICAL_SURFACE ( 'NONE', #5233, 3.000000000000002665 ) ;
#2059 = EDGE_LOOP ( 'NONE', ( #13155, #15519, #10163, #5816 ) ) ;
#2058 = ORIENTED_EDGE ( 'NONE', *, *, #21821, .T. ) ;
#2060 = EDGE_CURVE ( 'NONE', #11147, #10307, #20197, .T. ) ;
#2061 = ORIENTED_EDGE ( 'NONE', *, *, #9969, .F. ) ;
#2062 = EDGE_CURVE ( 'NONE', #15653, #23176, #8567, .T. ) ;
#2063 = VECTOR ( 'NONE', #18810, 1000.000000000000000 ) ;
#2064 = ADVANCED_FACE ( 'NONE', ( #14470 ), #17762, .T. ) ;
#2065 = ORIENTED_EDGE ( 'NONE', *, *, #2784, .F. ) ;
#2066 = ORIENTED_EDGE ( 'NONE', *, *, #20495, .F. ) ;
#2067 = VERTEX_POINT ( 'NONE', #13046 ) ;
#2068 = DIRECTION ( 'NONE',  ( -0.000000000000000000, -0.000000000000000000, 1.000000000000000000 ) ) ;
#2069 = CARTESIAN_POINT ( 'NONE',  ( -8.660254037844421049, 4.999999999999948486, -1.387778780781445676E-14 ) ) ;
#2070 = EDGE_CURVE ( 'NONE', #7007, #10462, #19988, .T. ) ;
#2071 = DIRECTION ( 'NONE',  ( 9.693522803355793065E-26, -5.963788443470848352E-28, -1.000000000000000000 ) ) ;
#2072 = ADVANCED_FACE ( 'NONE', ( #5996 ), #15152, .F. ) ;
#2073 = DIRECTION ( 'NONE',  ( -2.775557561562824791E-17, 0.000000000000000000, -1.000000000000000000 ) ) ;
#2074 = CARTESIAN_POINT ( 'NONE',  ( 5.599999999999991651, -6.249257483547704998E-31, 5.200000000000001066 ) ) ;
#2075 = CARTESIAN_POINT ( 'NONE',  ( 6.000000000291855429, -9.961476088449217059E-10, -5.999999999999998224 ) ) ;
#2076 = DIRECTION ( 'NONE',  ( 0.000000000000000000, 0.000000000000000000, -1.000000000000000000 ) ) ;
#2077 = EDGE_CURVE ( 'NONE', #8641, #18911, #11561, .T. ) ;
#2078 = CARTESIAN_POINT ( 'NONE',  ( 61.48996577904087957, -5.119475911334187224, -5.999999999999943157 ) ) ;
#2079 = CARTESIAN_POINT ( 'NONE',  ( -3.999999999708153453, 13.99999999900385106, -25.50000000000000000 ) ) ;
#2080 = DIRECTION ( 'NONE',  ( 0.000000000000000000, -6.938893903907237844E-15, -1.000000000000000000 ) ) ;
#2081 = CARTESIAN_POINT ( 'NONE',  ( -45.01801948466087566, 6.474873734152869709, 8.000000000000007105 ) ) ;
#2082 = DIRECTION ( 'NONE',  ( 0.000000000000000000, 0.000000000000000000, 1.000000000000000000 ) ) ;
#2083 = DIRECTION ( 'NONE',  ( -1.000000000000000000, 1.389842848855773151E-62, -2.013525853228507618E-32 ) ) ;
#2084 = PLANE ( 'NONE',  #14547 ) ;
#2085 = ORIENTED_EDGE ( 'NONE', *, *, #12867, .F. ) ;
#2086 = ORIENTED_EDGE ( 'NONE', *, *, #2342, .F. ) ;
#2087 = CARTESIAN_POINT ( 'NONE',  ( -5.688936712956119024, 36.29949271875472050, -28.48196112119369872 ) ) ;
#2088 = FACE_OUTER_BOUND ( 'NONE', #546, .T. ) ;
#2089 = VERTEX_POINT ( 'NONE', #13283 ) ;
#2090 = MECHANICAL_DESIGN_GEOMETRIC_PRESENTATION_REPRESENTATION (  '', ( #7610 ), #17491 ) ;
#2091 = DIRECTION ( 'NONE',  ( -1.000000000000000000, 0.000000000000000000, -4.336808689941968432E-16 ) ) ;
#2092 = EDGE_CURVE ( 'NONE', #17188, #8087, #7809, .T. ) ;
#2093 = DIRECTION ( 'NONE',  ( -7.860214984770699307E-18, 1.409037165336591006E-16, 1.000000000000000000 ) ) ;
#2094 = CARTESIAN_POINT ( 'NONE',  ( 4.175813232069149450, 2.061359961916364725, -3.570380186727398986 ) ) ;
#2095 = DIRECTION ( 'NONE',  ( 2.775557561562883647E-17, -3.652049423109057473E-16, 1.000000000000000000 ) ) ;
#2096 = CARTESIAN_POINT ( 'NONE',  ( 12.84999999999999964, -2.000000000000005329, -5.749999999999991118 ) ) ;
#2097 = VERTEX_POINT ( 'NONE', #7522 ) ;
#2098 = AXIS2_PLACEMENT_3D ( 'NONE', #16122, #18136, #7434 ) ;
#2099 = CARTESIAN_POINT ( 'NONE',  ( -4.000000000000052403, -2.309401076758560656, -5.000000000000000888 ) ) ;
#2100 = CARTESIAN_POINT ( 'NONE',  ( -43.46238456605036760, -4.919238815542504639, -8.000000000000062172 ) ) ;
#2101 = DIRECTION ( 'NONE',  ( 0.000000000000000000, -1.000000000000000000, 0.000000000000000000 ) ) ;
#2102 = EDGE_CURVE ( 'NONE', #13536, #6998, #4419, .T. ) ;
#2103 = DIRECTION ( 'NONE',  ( 1.000000000000000000, 0.000000000000000000, 0.000000000000000000 ) ) ;
#2104 = VECTOR ( 'NONE', #1291, 1000.000000000000000 ) ;
#2105 = CARTESIAN_POINT ( 'NONE',  ( -55.25320565519152893, 1.040834085586084257E-13, 8.000000000000035527 ) ) ;
#2106 = CARTESIAN_POINT ( 'NONE',  ( 86.02937988905577527, -11.02760560296348125, -5.999999999999991118 ) ) ;
#2107 = CARTESIAN_POINT ( 'NONE',  ( 3.958484000407791914, 2.327740518749039644, -2.968235154689956801 ) ) ;
#2108 = DIRECTION ( 'NONE',  ( 1.000000000000000000, -4.190823558986610327E-31, 1.733449886265890494E-32 ) ) ;
#2109 = EDGE_CURVE ( 'NONE', #12680, #1550, #1426, .T. ) ;
#2110 = CARTESIAN_POINT ( 'NONE',  ( 4.124214193018072905, 2.028338413290942110, -3.513185186763557066 ) ) ;
#2111 = AXIS2_PLACEMENT_3D ( 'NONE', #17977, #12552, #1844 ) ;
#2112 = SHAPE_DEFINITION_REPRESENTATION ( #15484, #1164 ) ;
#2113 = ORIENTED_EDGE ( 'NONE', *, *, #461, .F. ) ;
#2114 = AXIS2_PLACEMENT_3D ( 'NONE', #21381, #3259, #10764 ) ;
#2115 = ORIENTED_EDGE ( 'NONE', *, *, #17411, .T. ) ;
#2117 = ORIENTED_EDGE ( 'NONE', *, *, #5918, .F. ) ;
#2116 = VERTEX_POINT ( 'NONE', #2452 ) ;
#2118 = AXIS2_PLACEMENT_3D ( 'NONE', #12144, #15902, #14155 ) ;
#2119 = CARTESIAN_POINT ( 'NONE',  ( -3.200000000000091660, -6.938893903907228378E-14, 8.000000000000035527 ) ) ;
#2120 = CARTESIAN_POINT ( 'NONE',  ( 6.000000000291855429, -0.5000000009961480529, -36.44999999999999574 ) ) ;
#2121 = CARTESIAN_POINT ( 'NONE',  ( 7.551224464536113956, -11.87866898603340537, 7.234820221745447810 ) ) ;
#2122 = DIRECTION ( 'NONE',  ( 1.733449886265891589E-32, -4.190823558986610327E-31, 1.000000000000000000 ) ) ;
#2123 = DIRECTION ( 'NONE',  ( 1.000000000000000000, 1.424116703980846297E-16, -1.095779650622964657E-32 ) ) ;
#2124 = DIRECTION ( 'NONE',  ( 1.066786462891689527E-26, 6.656013887802287108E-31, 1.000000000000000000 ) ) ;
#2125 = DIRECTION ( 'NONE',  ( 0.000000000000000000, 1.000000000000000000, 0.000000000000000000 ) ) ;
#2126 = CARTESIAN_POINT ( 'NONE',  ( -50.65685424949274562, -2.700000000000125855, 8.000000000000062172 ) ) ;
#2127 =( BOUNDED_SURFACE ( )  B_SPLINE_SURFACE ( 3, 2, ( 
 ( #13391, #12069, #19148 ),
 ( #4558, #18927, #11733 ),
 ( #19259, #13747, #20929 ),
 ( #4795, #20575, #10202 ),
 ( #17371, #1052, #22452 ),
 ( #6685, #6342, #13857 ) ),
 .UNSPECIFIED., .F., .F., .F. ) 
 B_SPLINE_SURFACE_WITH_KNOTS ( ( 4, 2, 4 ),
 ( 3, 3 ),
 ( 0.01651999345535505592, 0.01858032176739835006, 0.02064065007944164767 ),
 ( 0.000000000000000000, 1.000000000000000000 ),
 .UNSPECIFIED. ) 
 GEOMETRIC_REPRESENTATION_ITEM ( )  RATIONAL_B_SPLINE_SURFACE ( (
 ( 1.000000000000000000, 0.8047781103519399126, 1.000000000000000000),
 ( 1.000000000000000000, 0.8123785825599758592, 1.000000000000000000),
 ( 1.000000000000000000, 0.8190671539794385225, 1.000000000000000000),
 ( 1.000000000000000000, 0.8192352254828778602, 1.000000000000000000),
 ( 1.000000000000000000, 0.8126129677216167302, 1.000000000000000000),
 ( 1.000000000000000000, 0.8047712537969725632, 1.000000000000000000) ) ) 
 REPRESENTATION_ITEM ( '' )  SURFACE ( )  );
#2128 = AXIS2_PLACEMENT_3D ( 'NONE', #16901, #17251, #6337 ) ;
#2129 = LINE ( 'NONE', #14497, #20800 ) ;
#2130 = LINE ( 'NONE', #16478, #444 ) ;
#2131 = DIRECTION ( 'NONE',  ( 0.000000000000000000, 0.000000000000000000, 1.000000000000000000 ) ) ;
#2132 = CIRCLE ( 'NONE', #645, 7.000000000000006217 ) ;
#2133 = CYLINDRICAL_SURFACE ( 'NONE', #17520, 4.749999999999986677 ) ;
#2134 = MECHANICAL_DESIGN_GEOMETRIC_PRESENTATION_REPRESENTATION (  '', ( #267 ), #1772 ) ;
#2135 = CARTESIAN_POINT ( 'NONE',  ( 8.195710046796573778, -2.011959044857176249, 6.570882465138042861 ) ) ;
#2136 = AXIS2_PLACEMENT_3D ( 'NONE', #16578, #13075, #18712 ) ;
#2137 = CARTESIAN_POINT ( 'NONE',  ( 2.591920818598158051E-16, 2.859595677584346074, -2.047034997319578498 ) ) ;
#2138 = CARTESIAN_POINT ( 'NONE',  ( 8.954763739086839536, 1.073360150760649390E-14, 6.678571428571445701 ) ) ;
#2139 = VERTEX_POINT ( 'NONE', #2100 ) ;
#2140 = ADVANCED_FACE ( 'NONE', ( #16905 ), #2223, .T. ) ;
#2141 = AXIS2_PLACEMENT_3D ( 'NONE', #5036, #12437, #3627 ) ;
#2143 = ORIENTED_EDGE ( 'NONE', *, *, #22541, .T. ) ;
#2142 = ORIENTED_EDGE ( 'NONE', *, *, #9809, .F. ) ;
#2144 = ORIENTED_EDGE ( 'NONE', *, *, #5082, .F. ) ;
#2146 = ORIENTED_EDGE ( 'NONE', *, *, #6980, .T. ) ;
#2145 = ORIENTED_EDGE ( 'NONE', *, *, #12997, .F. ) ;
#2147 = ORIENTED_EDGE ( 'NONE', *, *, #20616, .F. ) ;
#2148 = CIRCLE ( 'NONE', #6298, 0.5000000000000012212 ) ;
#2149 = ORIENTED_EDGE ( 'NONE', *, *, #14274, .F. ) ;
#2150 = DIRECTION ( 'NONE',  ( 0.000000000000000000, 0.000000000000000000, 1.000000000000000000 ) ) ;
#2151 = AXIS2_PLACEMENT_3D ( 'NONE', #13612, #17479, #13377 ) ;
#2152 = ORIENTED_EDGE ( 'NONE', *, *, #4473, .F. ) ;
#2153 = ORIENTED_EDGE ( 'NONE', *, *, #17447, .F. ) ;
#2154 = CYLINDRICAL_SURFACE ( 'NONE', #15549, 4.000000000000023981 ) ;
#2155 = CARTESIAN_POINT ( 'NONE',  ( 110.9706201109470811, -9.453020409440348715, -5.999999999999956479 ) ) ;
#2156 = AXIS2_PLACEMENT_3D ( 'NONE', #18344, #16552, #7636 ) ;
#2157 = EDGE_CURVE ( 'NONE', #746, #9743, #355, .T. ) ;
#2158 = CARTESIAN_POINT ( 'NONE',  ( 0.000000000000000000, 0.000000000000000000, 0.000000000000000000 ) ) ;
#2159 = CARTESIAN_POINT ( 'NONE',  ( -7.638377885296698366, -1.936221580213996374, 8.340398698103385300 ) ) ;
#2160 = VECTOR ( 'NONE', #21970, 1000.000000000000000 ) ;
#2161 = CIRCLE ( 'NONE', #9694, 0.5000000000000004441 ) ;
#2162 = DIRECTION ( 'NONE',  ( 0.000000000000000000, 0.000000000000000000, -1.000000000000000000 ) ) ;
#2163 = CARTESIAN_POINT ( 'NONE',  ( 3.951447005078452701, -2.357513599190993681, -2.916666666666662078 ) ) ;
#2164 = CYLINDRICAL_SURFACE ( 'NONE', #12544, 6.000000000000000000 ) ;
#2165 = DIRECTION ( 'NONE',  ( 0.000000000000000000, 0.000000000000000000, 1.000000000000000000 ) ) ;
#2166 = AXIS2_PLACEMENT_3D ( 'NONE', #15561, #8286, #22401 ) ;
#2167 = ADVANCED_FACE ( 'NONE', ( #11162 ), #13167, .F. ) ;
#2168 = CARTESIAN_POINT ( 'NONE',  ( 0.2499999999999967526, 1.250000000000042633, -17.00000000000000711 ) ) ;
#2169 = CIRCLE ( 'NONE', #13446, 2.500000000000006661 ) ;
#2170 = LINE ( 'NONE', #3707, #22791 ) ;
#2171 = AXIS2_PLACEMENT_3D ( 'NONE', #12179, #17600, #23264 ) ;
#2172 = EDGE_LOOP ( 'NONE', ( #20562, #16691, #3291, #6613 ) ) ;
#2173 = EDGE_CURVE ( 'NONE', #1520, #13097, #19438, .T. ) ;
#2174 = FACE_OUTER_BOUND ( 'NONE', #14632, .T. ) ;
#2176 = ORIENTED_EDGE ( 'NONE', *, *, #23022, .F. ) ;
#2175 = EDGE_LOOP ( 'NONE', ( #20129, #22994, #7714, #4335 ) ) ;
#2177 = CIRCLE ( 'NONE', #7459, 5.371010071662833063 ) ;
#2178 = ORIENTED_EDGE ( 'NONE', *, *, #5139, .F. ) ;
#2179 = VECTOR ( 'NONE', #21168, 1000.000000000000000 ) ;
#2180 = EDGE_CURVE ( 'NONE', #20512, #5232, #6304, .T. ) ;
#2181 = ORIENTED_EDGE ( 'NONE', *, *, #14586, .T. ) ;
#2182 = AXIS2_PLACEMENT_3D ( 'NONE', #11996, #13664, #17057 ) ;
#2183 = EDGE_CURVE ( 'NONE', #522, #22680, #12297, .T. ) ;
#2184 = ORIENTED_EDGE ( 'NONE', *, *, #17433, .F. ) ;
#2185 = EDGE_CURVE ( 'NONE', #11003, #11666, #6705, .T. ) ;
#2186 = ORIENTED_EDGE ( 'NONE', *, *, #21785, .T. ) ;
#2187 = CARTESIAN_POINT ( 'NONE',  ( 2.775557561562891351E-14, 2.999999999999999112, -12.50000000000001066 ) ) ;
#2188 = DIRECTION ( 'NONE',  ( 1.000000000000000000, 1.599800538956372742E-14, 3.854941057726199147E-16 ) ) ;
#2189 = STYLED_ITEM ( 'NONE', ( #15993 ), #18435 ) ;
#2190 = CARTESIAN_POINT ( 'NONE',  ( -6.000000000000047073, -4.800000000000006040, 8.000000000000090594 ) ) ;
#2191 = CARTESIAN_POINT ( 'NONE',  ( -45.56568542494955665, 0.5000000000000559552, -8.000000000000062172 ) ) ;
#2192 = DIRECTION ( 'NONE',  ( 0.000000000000000000, -1.000000000000000000, 0.000000000000000000 ) ) ;
#2193 = CARTESIAN_POINT ( 'NONE',  ( 5.551115123125782702E-14, 3.000000000000027089, 2.500000000000071498 ) ) ;
#2194 = DIRECTION ( 'NONE',  ( -9.693457064947022734E-26, 0.000000000000000000, 1.000000000000000000 ) ) ;
#2195 = EDGE_CURVE ( 'NONE', #22557, #6752, #7982, .T. ) ;
#2196 = EDGE_CURVE ( 'NONE', #5465, #195, #14566, .T. ) ;
#2197 = CYLINDRICAL_SURFACE ( 'NONE', #13937, 7.000000000000075495 ) ;
#2198 = CIRCLE ( 'NONE', #9730, 0.4999999999999995559 ) ;
#2199 = EDGE_CURVE ( 'NONE', #8317, #11002, #5565, .T. ) ;
#2200 = CARTESIAN_POINT ( 'NONE',  ( -1.442209863900529188, 4.971646688682866078, -7.500000000000002665 ) ) ;
#2201 = VECTOR ( 'NONE', #15333, 1000.000000000000114 ) ;
#2202 = LINE ( 'NONE', #5861, #3888 ) ;
#2203 = CARTESIAN_POINT ( 'NONE',  ( -12.84999999999998721, -12.50000000000002842, 5.750000000000060396 ) ) ;
#2204 =( NAMED_UNIT ( * ) SI_UNIT ( $, .STERADIAN. ) SOLID_ANGLE_UNIT ( ) );
#2205 = CARTESIAN_POINT ( 'NONE',  ( -2.000000000000015543, -3.464101615137743728, 0.000000000000000000 ) ) ;
#2206 = CARTESIAN_POINT ( 'NONE',  ( 22.49999999999998224, 2.000000000000001776, -0.2500000000000210387 ) ) ;
#2207 = EDGE_CURVE ( 'NONE', #13979, #2913, #6107, .T. ) ;
#2208 =( GEOMETRIC_REPRESENTATION_CONTEXT ( 3 ) GLOBAL_UNCERTAINTY_ASSIGNED_CONTEXT ( ( #9789 ) ) GLOBAL_UNIT_ASSIGNED_CONTEXT ( ( #15597, #17476, #8547 ) ) REPRESENTATION_CONTEXT ( 'NONE', 'WORKASPACE' ) );
#2209 = EDGE_CURVE ( 'NONE', #18644, #14732, #20963, .T. ) ;
#2210 = ORIENTED_EDGE ( 'NONE', *, *, #19749, .T. ) ;
#2211 = AXIS2_PLACEMENT_3D ( 'NONE', #21190, #11761, #2833 ) ;
#2212 = EDGE_CURVE ( 'NONE', #10962, #22329, #19836, .T. ) ;
#2213 = DIRECTION ( 'NONE',  ( -0.7313537016191794526, -0.6819983600624889286, -4.403559511741029625E-16 ) ) ;
#2214 = DIRECTION ( 'NONE',  ( 1.333893503340774882E-15, 2.778352770573747380E-17, 1.000000000000000000 ) ) ;
#2215 = ORIENTED_EDGE ( 'NONE', *, *, #1528, .T. ) ;
#2216 = AXIS2_PLACEMENT_3D ( 'NONE', #8310, #9965, #4539 ) ;
#2217 = DIRECTION ( 'NONE',  ( -1.066786462891689527E-26, -6.656013887802287108E-31, -1.000000000000000000 ) ) ;
#2218 = DIRECTION ( 'NONE',  ( -1.333893503340774882E-15, -2.778352770573747380E-17, -1.000000000000000000 ) ) ;
#2219 = CARTESIAN_POINT ( 'NONE',  ( 8.195710046796559567, -11.98804095514285173, 6.570882465138090822 ) ) ;
#2220 = CARTESIAN_POINT ( 'NONE',  ( -45.56568542494949980, -2.108831175456918228, -7.500000000000007105 ) ) ;
#2221 = LINE ( 'NONE', #15463, #7149 ) ;
#2222 = CARTESIAN_POINT ( 'NONE',  ( 3.000000000291852764, 42.99999999900385461, -29.00000000000000355 ) ) ;
#2223 = PLANE ( 'NONE',  #22844 ) ;
#2224 = ADVANCED_FACE ( 'NONE', ( #4686 ), #5585, .T. ) ;
#2225 = CARTESIAN_POINT ( 'NONE',  ( 5.100000000000000533, 1.758911592640616865E-31, 5.200000000000004619 ) ) ;
#2226 = CARTESIAN_POINT ( 'NONE',  ( 77.42435809754137210, -6.999999999999811706, 6.500000000000081712 ) ) ;
#2227 = MECHANICAL_DESIGN_GEOMETRIC_PRESENTATION_REPRESENTATION (  '', ( #357 ), #13500 ) ;
#2228 = CARTESIAN_POINT ( 'NONE',  ( 7.856071383949645437, -13.95231939088842488, 7.015054140272347638 ) ) ;
#2229 = DIRECTION ( 'NONE',  ( -0.000000000000000000, 1.000000000000000000, -0.000000000000000000 ) ) ;
#2230 = PLANE ( 'NONE',  #10685 ) ;
#2231 = CARTESIAN_POINT ( 'NONE',  ( 119.9981234580896796, -4.453056000818161664, 6.000000000000123457 ) ) ;
#2232 = CARTESIAN_POINT ( 'NONE',  ( 0.3198814748697104693, 4.434118497892227673, -0.3507732604232764451 ) ) ;
#2233 = AXIS2_PLACEMENT_3D ( 'NONE', #1790, #10945, #16126 ) ;
#2234 = DIRECTION ( 'NONE',  ( 1.000000000000000000, 2.365532012695631919E-16, -4.455085290576773719E-15 ) ) ;
#2235 = EDGE_CURVE ( 'NONE', #19565, #12056, #7444, .T. ) ;
#2236 = PRODUCT_CONTEXT ( 'NONE', #4265, 'mechanical' ) ;
#2237 = AXIS2_PLACEMENT_3D ( 'NONE', #17046, #959, #8123 ) ;
#2238 = VERTEX_POINT ( 'NONE', #15258 ) ;
#2239 = EDGE_CURVE ( 'NONE', #4523, #4400, #2177, .T. ) ;
#2240 = PRESENTATION_LAYER_ASSIGNMENT (  '', '', ( #9018 ) ) ;
#2242 = VERTEX_POINT ( 'NONE', #13512 ) ;
#2241 = ORIENTED_EDGE ( 'NONE', *, *, #19442, .F. ) ;
#2243 = CARTESIAN_POINT ( 'NONE',  ( -0.1410422978106479486, 4.700232962125154401, -3.687027686973645135 ) ) ;
#2244 = B_SPLINE_CURVE_WITH_KNOTS ( 'NONE', 3,
 ( #6710, #1077, #3060, #4928, #12096, #17395, #20947, #6949 ),
 .UNSPECIFIED., .F., .F.,
 ( 4, 2, 2, 4 ),
 ( 1.379105163401561640E-16, 0.001256837924491785441, 0.001885256886737605954, 0.002513675848983426466 ),
 .UNSPECIFIED. ) ;
#2245 = DIRECTION ( 'NONE',  ( 1.550910762415566494E-16, 1.000000000000000000, -8.135128085091684243E-31 ) ) ;
#2246 = CARTESIAN_POINT ( 'NONE',  ( 7.971461718369340588, -11.76779483280627048, 7.625732677302466733 ) ) ;
#2247 = ORIENTED_EDGE ( 'NONE', *, *, #14877, .T. ) ;
#2248 = DIRECTION ( 'NONE',  ( 2.013525853228508439E-32, 6.779273404243028164E-31, -1.000000000000000000 ) ) ;
#2249 = DIRECTION ( 'NONE',  ( 0.000000000000000000, -1.000000000000000000, 0.000000000000000000 ) ) ;
#2250 = CARTESIAN_POINT ( 'NONE',  ( 1.387778780781445676E-14, 4.618802153517020059, -5.242734410091827613 ) ) ;
#2251 = DIRECTION ( 'NONE',  ( -1.000000000000000000, 1.389842848855773367E-62, -2.013525853228507892E-32 ) ) ;
#2252 = DIRECTION ( 'NONE',  ( -0.6819983600624998088, -0.7313537016191693496, 0.000000000000000000 ) ) ;
#2253 = DIRECTION ( 'NONE',  ( 3.241725282392603095E-30, 1.000000000000000000, -2.218671295934100958E-31 ) ) ;
#2254 = CARTESIAN_POINT ( 'NONE',  ( 4.211140560182139225, 2.431303136016540911, -3.745885042887430405 ) ) ;
#2255 = CARTESIAN_POINT ( 'NONE',  ( 29.00000000029184832, 16.99999999900385461, -29.00000000000000355 ) ) ;
#2256 = FILL_AREA_STYLE_COLOUR ( '', #4776 ) ;
#2257 = DIRECTION ( 'NONE',  ( -1.000000000000000000, 0.000000000000000000, 0.000000000000000000 ) ) ;
#2258 = LINE ( 'NONE', #18611, #10431 ) ;
#2259 = CARTESIAN_POINT ( 'NONE',  ( 0.02993401039713806250, 2.688325911136462132, -2.343682934607768331 ) ) ;
#2260 = CARTESIAN_POINT ( 'NONE',  ( 7.748687480237993697, -0.2688970177183283572, 8.040801957829158297 ) ) ;
#2261 = EDGE_CURVE ( 'NONE', #4634, #9218, #7087, .T. ) ;
#2262 = VERTEX_POINT ( 'NONE', #1283 ) ;
#2263 = SHAPE_DEFINITION_REPRESENTATION ( #20767, #19450 ) ;
#2265 = ORIENTED_EDGE ( 'NONE', *, *, #12537, .T. ) ;
#2264 = VERTEX_POINT ( 'NONE', #6577 ) ;
#2266 = UNCERTAINTY_MEASURE_WITH_UNIT (LENGTH_MEASURE( 1.000000000000000082E-05 ), #14864, 'distance_accuracy_value', 'NONE');
#2267 = ADVANCED_FACE ( 'NONE', ( #8566 ), #22923, .T. ) ;
#2268 = ORIENTED_EDGE ( 'NONE', *, *, #21470, .T. ) ;
#2269 = ORIENTED_EDGE ( 'NONE', *, *, #8952, .T. ) ;
#2271 = ORIENTED_EDGE ( 'NONE', *, *, #5661, .F. ) ;
#2270 = ORIENTED_EDGE ( 'NONE', *, *, #13585, .T. ) ;
#2272 = AXIS2_PLACEMENT_3D ( 'NONE', #42, #10841, #2012 ) ;
#2273 = EDGE_LOOP ( 'NONE', ( #2521, #9741, #12678, #4333 ) ) ;
#2274 = ORIENTED_EDGE ( 'NONE', *, *, #13394, .T. ) ;
#2275 = DIRECTION ( 'NONE',  ( -1.454462294001240516E-30, -1.000000000000000000, -0.000000000000000000 ) ) ;
#2276 = ORIENTED_EDGE ( 'NONE', *, *, #9187, .T. ) ;
#2277 = ORIENTED_EDGE ( 'NONE', *, *, #12230, .T. ) ;
#2278 = DIRECTION ( 'NONE',  ( -2.220446049250313081E-16, 1.000000000000000000, -7.025792437124636392E-31 ) ) ;
#2279 = DIRECTION ( 'NONE',  ( 2.013525853228507892E-32, 6.902532920683810383E-31, -1.000000000000000000 ) ) ;
#2280 = CARTESIAN_POINT ( 'NONE',  ( -6.000000000000088818, 7.499999999999958256, 8.000000000000035527 ) ) ;
#2281 = ADVANCED_FACE ( 'NONE', ( #22568 ), #4903, .T. ) ;
#2282 = CARTESIAN_POINT ( 'NONE',  ( 0.02993401039715375481, 2.688325911136459911, -2.343682934607804746 ) ) ;
#2283 = FACE_OUTER_BOUND ( 'NONE', #10429, .T. ) ;
#2284 = DIRECTION ( 'NONE',  ( 0.000000000000000000, 0.000000000000000000, -1.000000000000000000 ) ) ;
#2285 = DIRECTION ( 'NONE',  ( 0.000000000000000000, 1.000000000000000000, -6.383782391594650107E-16 ) ) ;
#2286 = CARTESIAN_POINT ( 'NONE',  ( 30.00000000029184832, -9.961476088449217059E-10, -8.549999999999997158 ) ) ;
#2287 = AXIS2_PLACEMENT_3D ( 'NONE', #10010, #15175, #20361 ) ;
#2288 = DIRECTION ( 'NONE',  ( 1.000000000000000000, 0.000000000000000000, 0.000000000000000000 ) ) ;
#2289 = ORIENTED_EDGE ( 'NONE', *, *, #5634, .T. ) ;
#2290 =( NAMED_UNIT ( * ) SI_UNIT ( $, .STERADIAN. ) SOLID_ANGLE_UNIT ( ) );
#2292 = VERTEX_POINT ( 'NONE', #11966 ) ;
#2291 = ORIENTED_EDGE ( 'NONE', *, *, #18696, .F. ) ;
#2293 = VERTEX_POINT ( 'NONE', #3164 ) ;
#2294 = VERTEX_POINT ( 'NONE', #10100 ) ;
#2295 = ORIENTED_EDGE ( 'NONE', *, *, #10778, .F. ) ;
#2296 = CARTESIAN_POINT ( 'NONE',  ( -91.02295700146262902, 6.938893903907228378E-15, 6.338518968055040226 ) ) ;
#2297 = CIRCLE ( 'NONE', #75, 0.5000000000000038858 ) ;
#2298 = VECTOR ( 'NONE', #19851, 1000.000000000000000 ) ;
#2299 = DIRECTION ( 'NONE',  ( 1.333893503340774882E-15, 2.778352770573747380E-17, 1.000000000000000000 ) ) ;
#2300 = ORIENTED_EDGE ( 'NONE', *, *, #23059, .F. ) ;
#2301 = FACE_BOUND ( 'NONE', #21032, .T. ) ;
#2302 = EDGE_CURVE ( 'NONE', #5891, #2238, #938, .T. ) ;
#2303 = CYLINDRICAL_SURFACE ( 'NONE', #18883, 2.500000000000006661 ) ;
#2304 = CARTESIAN_POINT ( 'NONE',  ( 7.938566201357266650, 4.882486540518886642, 1.249999999999969580 ) ) ;
#2305 = LINE ( 'NONE', #908, #4186 ) ;
#2306 = CARTESIAN_POINT ( 'NONE',  ( -8.165409815605745081, -11.99182595524112571, 6.581206704444157118 ) ) ;
#2307 = CARTESIAN_POINT ( 'NONE',  ( -7.490952241692505176, -13.34551170378494689, 8.992386117842826820 ) ) ;
#2308 = DIRECTION ( 'NONE',  ( -2.013525853219289976E-32, 5.941108692445745160E-30, 1.000000000000000000 ) ) ;
#2309 = ADVANCED_FACE ( 'NONE', ( #17493 ), #2127, .F. ) ;
#2310 = CARTESIAN_POINT ( 'NONE',  ( -2.100000000000000089, 3.008176102356893744E-15, -4.694516984716114116 ) ) ;
#2311 = APPLICATION_CONTEXT ( 'automotive_design' ) ;
#2313 = EDGE_CURVE ( 'NONE', #22269, #6361, #17197, .T. ) ;
#2312 = FACE_OUTER_BOUND ( 'NONE', #10227, .T. ) ;
#2314 = FILL_AREA_STYLE_COLOUR ( '', #14588 ) ;
#2315 = CARTESIAN_POINT ( 'NONE',  ( -50.65685424949275983, -0.5000000000000905942, -8.000000000000007105 ) ) ;
#2317 = AXIS2_PLACEMENT_3D ( 'NONE', #19356, #17586, #13603 ) ;
#2316 = CARTESIAN_POINT ( 'NONE',  ( 4.158921444904714271, -2.089933220600045605, -3.500000000000009326 ) ) ;
#2318 = CIRCLE ( 'NONE', #17336, 0.4999999999999994449 ) ;
#2319 = VERTEX_POINT ( 'NONE', #10674 ) ;
#2320 = ORIENTED_EDGE ( 'NONE', *, *, #20768, .T. ) ;
#2321 = CARTESIAN_POINT ( 'NONE',  ( 22.49999999999996092, 4.500000000000073719, -17.74999999999998224 ) ) ;
#2322 = EDGE_CURVE ( 'NONE', #17450, #4649, #1808, .T. ) ;
#2323 = ADVANCED_FACE ( 'NONE', ( #10556 ), #1507, .F. ) ;
#2324 = DIRECTION ( 'NONE',  ( 5.551115123561405253E-17, 1.000000000000000000, -5.963788443470795439E-28 ) ) ;
#2325 = ORIENTED_EDGE ( 'NONE', *, *, #16245, .T. ) ;
#2326 = DIRECTION ( 'NONE',  ( -1.000000000000000000, -4.440892098500626162E-16, 5.551115123125782702E-16 ) ) ;
#2327 = DIRECTION ( 'NONE',  ( -1.134196829589822256E-15, -2.220446049250322449E-16, 1.000000000000000000 ) ) ;
#2328 = LINE ( 'NONE', #14915, #12088 ) ;
#2329 = EDGE_CURVE ( 'NONE', #14364, #16088, #4812, .T. ) ;
#2330 = DIRECTION ( 'NONE',  ( 1.000000000000000000, 3.254448077276381206E-32, 1.066788928082016908E-26 ) ) ;
#2331 = CARTESIAN_POINT ( 'NONE',  ( 108.2426266706970779, -6.527605602963587828, 6.000000000000109246 ) ) ;
#2332 = AXIS2_PLACEMENT_3D ( 'NONE', #5854, #16756, #9373 ) ;
#2333 = DIRECTION ( 'NONE',  ( 1.000000000000000000, 0.000000000000000000, 0.000000000000000000 ) ) ;
#2334 = CARTESIAN_POINT ( 'NONE',  ( -6.000000000000088818, 7.999999999999958256, 8.000000000000035527 ) ) ;
#2335 = AXIS2_PLACEMENT_3D ( 'NONE', #17855, #17973, #21402 ) ;
#2336 = CARTESIAN_POINT ( 'NONE',  ( 109.3164911904586916, -11.67918431276163105, -6.000000000000060396 ) ) ;
#2337 = CARTESIAN_POINT ( 'NONE',  ( 6.999999995237020656, -13.21736471697188797, 9.233045673661203878 ) ) ;
#2338 = DIRECTION ( 'NONE',  ( -0.000000000000000000, -0.000000000000000000, 1.000000000000000000 ) ) ;
#2339 = ADVANCED_FACE ( 'NONE', ( #21275 ), #21736, .T. ) ;
#2340 = CARTESIAN_POINT ( 'NONE',  ( -1.734723475976807094E-14, 2.000000000000001776, -17.00000000000000711 ) ) ;
#2341 = CARTESIAN_POINT ( 'NONE',  ( 3.806834918298642290, -9.107298248878237246E-15, -3.500000000000012434 ) ) ;
#2342 = EDGE_CURVE ( 'NONE', #14430, #1004, #14213, .T. ) ;
#2343 = CIRCLE ( 'NONE', #13978, 5.371010071662833063 ) ;
#2344 = CARTESIAN_POINT ( 'NONE',  ( 116.8476484622115805, -8.074585193523331483, -5.999999999999956479 ) ) ;
#2345 = APPLICATION_PROTOCOL_DEFINITION ( 'draft international standard', 'automotive_design', 1998, #10248 ) ;
#2346 = ORIENTED_EDGE ( 'NONE', *, *, #1783, .F. ) ;
#2347 = AXIS2_PLACEMENT_3D ( 'NONE', #6449, #1045, #11728 ) ;
#2348 = AXIS2_PLACEMENT_3D ( 'NONE', #21126, #14297, #4995 ) ;
#2349 = EDGE_CURVE ( 'NONE', #93, #10626, #10824, .T. ) ;
#2350 = AXIS2_PLACEMENT_3D ( 'NONE', #1158, #2800, #11849 ) ;
#2351 = ADVANCED_FACE ( 'NONE', ( #23040 ), #7160, .F. ) ;
#2353 = ORIENTED_EDGE ( 'NONE', *, *, #12867, .T. ) ;
#2352 = EDGE_LOOP ( 'NONE', ( #3577, #13267, #15281, #21360, #3708, #9622 ) ) ;
#2354 = CARTESIAN_POINT ( 'NONE',  ( -6.000000000000143885, 1.999999999999960032, 8.000000000000062172 ) ) ;
#2355 = CARTESIAN_POINT ( 'NONE',  ( 37.29045043747246524, 0.08880391167994924895, -2.421762079371568621 ) ) ;
#2356 = DIRECTION ( 'NONE',  ( -1.858632295689435609E-16, -1.000000000000000000, 0.000000000000000000 ) ) ;
#2357 = VERTEX_POINT ( 'NONE', #12661 ) ;
#2358 = DIRECTION ( 'NONE',  ( 0.000000000000000000, 0.000000000000000000, 1.000000000000000000 ) ) ;
#2359 = EDGE_CURVE ( 'NONE', #6825, #16331, #3277, .T. ) ;
#2360 = CARTESIAN_POINT ( 'NONE',  ( -12.85000000000002807, -13.50000000000003020, 6.250000000000033751 ) ) ;
#2361 = CARTESIAN_POINT ( 'NONE',  ( 4.132952817037863547, -2.031684012687259955, 3.518979934899748141 ) ) ;
#2362 = CARTESIAN_POINT ( 'NONE',  ( 0.2262162651715079187, -0.5999999999999898748, -3.877538419241197243 ) ) ;
#2363 = FACE_OUTER_BOUND ( 'NONE', #13769, .T. ) ;
#2364 = AXIS2_PLACEMENT_3D ( 'NONE', #14718, #13078, #2598 ) ;
#2365 = CARTESIAN_POINT ( 'NONE',  ( 42.00000000000014921, 10.49999999999999822, -12.50000000000005329 ) ) ;
#2366 = CIRCLE ( 'NONE', #5393, 2.500000000000015543 ) ;
#2367 = FACE_OUTER_BOUND ( 'NONE', #14508, .T. ) ;
#2368 = AXIS2_PLACEMENT_3D ( 'NONE', #16983, #8064, #20665 ) ;
#2369 = CARTESIAN_POINT ( 'NONE',  ( 57.49335071782248008, -0.7089083427137543580, 6.500000000000088818 ) ) ;
#2370 = CONICAL_SURFACE ( 'NONE', #17389, 4.000000000000000000, 1.047197551196595855 ) ;
#2371 = CARTESIAN_POINT ( 'NONE',  ( 4.630153689607052314, 6.577590292450120328E-16, 5.371010071662848162 ) ) ;
#2372 = CARTESIAN_POINT ( 'NONE',  ( -50.65685424949270299, 7.200000000000025935, 7.500000000000062172 ) ) ;
#2373 = CARTESIAN_POINT ( 'NONE',  ( 4.175813232069142344, 2.061359961916371830, 3.570380186727395433 ) ) ;
#2374 = FACE_OUTER_BOUND ( 'NONE', #5466, .T. ) ;
#2375 = EDGE_LOOP ( 'NONE', ( #6187, #5584, #1906, #1569 ) ) ;
#2376 = PRESENTATION_STYLE_ASSIGNMENT (( #20273 ) ) ;
#2378 = ORIENTED_EDGE ( 'NONE', *, *, #15996, .T. ) ;
#2377 = ORIENTED_EDGE ( 'NONE', *, *, #9962, .T. ) ;
#2379 = ORIENTED_EDGE ( 'NONE', *, *, #7246, .T. ) ;
#2380 = EDGE_LOOP ( 'NONE', ( #13614, #88, #18770 ) ) ;
#2381 = AXIS2_PLACEMENT_3D ( 'NONE', #1956, #9154, #16314 ) ;
#2383 = ORIENTED_EDGE ( 'NONE', *, *, #4311, .T. ) ;
#2382 = VERTEX_POINT ( 'NONE', #21403 ) ;
#2384 = AXIS2_PLACEMENT_3D ( 'NONE', #20464, #818, #15260 ) ;
#2385 = B_SPLINE_CURVE_WITH_KNOTS ( 'NONE', 3,
 ( #23157, #6918, #3158, #5267 ),
 .UNSPECIFIED., .F., .F.,
 ( 4, 4 ),
 ( 2.380735702043749618E-07, 0.002775112046897000757 ),
 .UNSPECIFIED. ) ;
#2386 = EDGE_LOOP ( 'NONE', ( #18996, #18444, #16291, #5485 ) ) ;
#2387 = CONICAL_SURFACE ( 'NONE', #15529, 4.000000000000000000, 1.047197551196595855 ) ;
#2388 = DIRECTION ( 'NONE',  ( 0.000000000000000000, 0.000000000000000000, -1.000000000000000000 ) ) ;
#2389 = AXIS2_PLACEMENT_3D ( 'NONE', #22561, #4553, #2801 ) ;
#2390 = ORIENTED_EDGE ( 'NONE', *, *, #3134, .T. ) ;
#2391 = AXIS2_PLACEMENT_3D ( 'NONE', #5990, #2326, #19981 ) ;
#2392 = ORIENTED_EDGE ( 'NONE', *, *, #9910, .F. ) ;
#2393 = CIRCLE ( 'NONE', #14786, 0.5000000000000028866 ) ;
#2394 = DIRECTION ( 'NONE',  ( -2.013525853228507892E-32, -6.902532920683810383E-31, 1.000000000000000000 ) ) ;
#2395 = CARTESIAN_POINT ( 'NONE',  ( 0.000000000000000000, 0.000000000000000000, -0.3080913168122707546 ) ) ;
#2396 = EDGE_CURVE ( 'NONE', #9669, #13984, #2561, .T. ) ;
#2397 = FACE_OUTER_BOUND ( 'NONE', #21427, .T. ) ;
#2398 = CARTESIAN_POINT ( 'NONE',  ( 7.499999999999978684, -12.60977222864647196, 9.250000000000049738 ) ) ;
#2399 = DIRECTION ( 'NONE',  ( -5.551115123125782702E-16, -1.201780285297635172E-31, 1.000000000000000000 ) ) ;
#2400 = DIRECTION ( 'NONE',  ( 1.858632295689435609E-16, 1.000000000000000000, 0.000000000000000000 ) ) ;
#2401 = CARTESIAN_POINT ( 'NONE',  ( 4.113620667976075396, -1.749999999999998002, -2.375000000000002220 ) ) ;
#2402 = CARTESIAN_POINT ( 'NONE',  ( -95.20000000000055707, -3.200000000000064126, -2.000000000000001776 ) ) ;
#2403 = EDGE_CURVE ( 'NONE', #17189, #18558, #15703, .T. ) ;
#2404 = PLANE ( 'NONE',  #19448 ) ;
#2405 = AXIS2_PLACEMENT_3D ( 'NONE', #5125, #12286, #12409 ) ;
#2406 = CIRCLE ( 'NONE', #14045, 6.500000000000023981 ) ;
#2407 = CIRCLE ( 'NONE', #8815, 7.500000000000001776 ) ;
#2408 = EDGE_LOOP ( 'NONE', ( #9819, #16490, #3078, #11320, #18097 ) ) ;
#2409 = CARTESIAN_POINT ( 'NONE',  ( 0.000000000000000000, 0.000000000000000000, 3.469446951953614189E-15 ) ) ;
#2411 = ORIENTED_EDGE ( 'NONE', *, *, #17578, .F. ) ;
#2410 = ORIENTED_EDGE ( 'NONE', *, *, #2903, .T. ) ;
#2412 = ORIENTED_EDGE ( 'NONE', *, *, #7948, .T. ) ;
#2413 = ORIENTED_EDGE ( 'NONE', *, *, #7152, .F. ) ;
#2414 = ORIENTED_EDGE ( 'NONE', *, *, #22450, .F. ) ;
#2415 = EDGE_LOOP ( 'NONE', ( #20282, #16350, #16925, #203, #3355, #16891 ) ) ;
#2416 = DIRECTION ( 'NONE',  ( -0.7313537016191734574, 0.6819983600624954789, -3.733258675956565293E-18 ) ) ;
#2417 = AXIS2_PLACEMENT_3D ( 'NONE', #10499, #19435, #18141 ) ;
#2418 = AXIS2_PLACEMENT_3D ( 'NONE', #11665, #18848, #11556 ) ;
#2419 = CIRCLE ( 'NONE', #9935, 0.5000000000000038858 ) ;
#2420 = PLANE ( 'NONE',  #10240 ) ;
#2421 = VERTEX_POINT ( 'NONE', #8913 ) ;
#2422 = LINE ( 'NONE', #16521, #22628 ) ;
#2423 = CARTESIAN_POINT ( 'NONE',  ( 24.99999999999995737, 2.000000000000001776, -16.99999999999999289 ) ) ;
#2424 = CARTESIAN_POINT ( 'NONE',  ( -57.28378781036000333, 0.5000000000000905942, 8.541666666666698049 ) ) ;
#2425 = CARTESIAN_POINT ( 'NONE',  ( -7.216878364870317419, 5.000000000000001776, -2.499999999999978240 ) ) ;
#2426 = CARTESIAN_POINT ( 'NONE',  ( 4.132952817037863547, 4.063368025374527015, 0.000000000000000000 ) ) ;
#2427 = CARTESIAN_POINT ( 'NONE',  ( -8.438463404362648745, -2.001835333048896715, 6.398712851742144103 ) ) ;
#2428 = CARTESIAN_POINT ( 'NONE',  ( 36.00000000029184832, -9.961476088449217059E-10, -26.50000000000000000 ) ) ;
#2429 = B_SPLINE_CURVE_WITH_KNOTS ( 'NONE', 3,
 ( #4016, #266, #14845, #22018, #20029, #1901 ),
 .UNSPECIFIED., .F., .F.,
 ( 4, 2, 4 ),
 ( 0.002336974151641522165, 0.003500975885716451491, 0.004664977619791380384 ),
 .UNSPECIFIED. ) ;
#2430 = LINE ( 'NONE', #20210, #22685 ) ;
#2431 = LINE ( 'NONE', #5744, #249 ) ;
#2432 = AXIS2_PLACEMENT_3D ( 'NONE', #14001, #5426, #1419 ) ;
#2433 = ADVANCED_BREP_SHAPE_REPRESENTATION ( '', ( #13118, #22115 ), #12003 ) ;
#2434 = SURFACE_STYLE_USAGE ( .BOTH. , #18325 ) ;
#2435 = CARTESIAN_POINT ( 'NONE',  ( 108.2426266706970637, -11.02760560296359138, 5.999999999999984901 ) ) ;
#2436 = AXIS2_PLACEMENT_3D ( 'NONE', #5086, #19320, #17907 ) ;
#2437 = CARTESIAN_POINT ( 'NONE',  ( 4.086375874528099139, -2.103253014742889171, -3.500000000000010214 ) ) ;
#2438 = ORIENTED_EDGE ( 'NONE', *, *, #6240, .T. ) ;
#2439 = EDGE_CURVE ( 'NONE', #12159, #20325, #5029, .T. ) ;
#2440 = EDGE_LOOP ( 'NONE', ( #2874, #16973, #17073, #19665 ) ) ;
#2441 = ORIENTED_EDGE ( 'NONE', *, *, #16109, .T. ) ;
#2442 = ORIENTED_EDGE ( 'NONE', *, *, #22740, .F. ) ;
#2443 = LINE ( 'NONE', #4678, #6493 ) ;
#2444 = CARTESIAN_POINT ( 'NONE',  ( -4.000000000000004441, -1.549102112939104714, -5.442104661404059129 ) ) ;
#2445 = ORIENTED_EDGE ( 'NONE', *, *, #7108, .T. ) ;
#2446 = FACE_OUTER_BOUND ( 'NONE', #4526, .T. ) ;
#2447 = CARTESIAN_POINT ( 'NONE',  ( 1.200000000000006617, -0.5999999999999894307, -4.749999999999948486 ) ) ;
#2448 = CARTESIAN_POINT ( 'NONE',  ( -6.000000000000074607, 1.999999999999960032, 7.500000000000062172 ) ) ;
#2449 = VECTOR ( 'NONE', #22347, 1000.000000000000000 ) ;
#2450 = AXIS2_PLACEMENT_3D ( 'NONE', #486, #22586, #20713 ) ;
#2451 = DIRECTION ( 'NONE',  ( -3.885780586188016830E-16, -4.437342591868156373E-31, 1.000000000000000000 ) ) ;
#2452 = CARTESIAN_POINT ( 'NONE',  ( -12.84999999999999964, 0.000000000000000000, -2.550000000000000711 ) ) ;
#2453 = CARTESIAN_POINT ( 'NONE',  ( 42.00000000000020606, -1.387778780781445676E-14, -0.4999999999999449329 ) ) ;
#2454 = DIRECTION ( 'NONE',  ( -0.000000000000000000, -0.000000000000000000, 1.000000000000000000 ) ) ;
#2455 = CARTESIAN_POINT ( 'NONE',  ( -7.000000000000006217, -8.000000000000017764, 10.24999999999999467 ) ) ;
#2456 = CARTESIAN_POINT ( 'NONE',  ( -50.65685424949267457, -7.200000000000049916, 7.500000000000047962 ) ) ;
#2457 = FACE_OUTER_BOUND ( 'NONE', #1299, .T. ) ;
#2458 = DIRECTION ( 'NONE',  ( 3.885780586188016830E-16, 4.437342591868156373E-31, -1.000000000000000000 ) ) ;
#2459 = EDGE_CURVE ( 'NONE', #19105, #20271, #10443, .T. ) ;
#2460 = CARTESIAN_POINT ( 'NONE',  ( 4.086262629614027198, -1.979770830881093513, -3.570936333571106847 ) ) ;
#2461 = CIRCLE ( 'NONE', #7000, 3.000000000000002665 ) ;
#2462 = ORIENTED_EDGE ( 'NONE', *, *, #21922, .T. ) ;
#2463 = EDGE_CURVE ( 'NONE', #3085, #7197, #14612, .T. ) ;
#2464 = ORIENTED_EDGE ( 'NONE', *, *, #5341, .T. ) ;
#2467 = ORIENTED_EDGE ( 'NONE', *, *, #18247, .T. ) ;
#2466 = ADVANCED_FACE ( 'NONE', ( #12550, #12192, #3618 ), #10784, .T. ) ;
#2465 = ORIENTED_EDGE ( 'NONE', *, *, #5784, .T. ) ;
#2468 = ADVANCED_FACE ( 'NONE', ( #9029 ), #15359, .T. ) ;
#2469 = LINE ( 'NONE', #6127, #2740 ) ;
#2470 = EDGE_CURVE ( 'NONE', #13557, #17638, #8665, .T. ) ;
#2471 = CARTESIAN_POINT ( 'NONE',  ( 0.9337610948747031570, -1.709055945004938293, -4.750000000000025757 ) ) ;
#2472 = VECTOR ( 'NONE', #9416, 1000.000000000000000 ) ;
#2473 = ORIENTED_EDGE ( 'NONE', *, *, #16535, .F. ) ;
#2474 = DIRECTION ( 'NONE',  ( 0.1556420233463076119, 0.000000000000000000, 0.9878135252003121813 ) ) ;
#2475 = CARTESIAN_POINT ( 'NONE',  ( -5.560781378645605066, 7.099763649701009246E-15, -4.000000000000007994 ) ) ;
#2476 = CARTESIAN_POINT ( 'NONE',  ( 4.104070371397483541, -2.023683613428369110, 3.505122836902506922 ) ) ;
#2477 = CARTESIAN_POINT ( 'NONE',  ( -5.498446330623520062, 36.40058408549440117, -16.39859714349349673 ) ) ;
#2478 = DIRECTION ( 'NONE',  ( 1.000000000000000000, 1.479114197289397135E-31, -7.395570986446975166E-31 ) ) ;
#2479 = CARTESIAN_POINT ( 'NONE',  ( 0.1388410611045837739, 3.710337782247994820, 0.5735064479039461149 ) ) ;
#2480 = CARTESIAN_POINT ( 'NONE',  ( -1.442209863900557387, 4.971646688682839432, 7.500000000000007105 ) ) ;
#2481 = CARTESIAN_POINT ( 'NONE',  ( 124.5000000000019469, -6.500000000000061284, 4.857225732735059864E-14 ) ) ;
#2482 = ADVANCED_FACE ( 'NONE', ( #12312 ), #17616, .T. ) ;
#2483 = ADVANCED_FACE ( 'NONE', ( #16758 ), #16106, .T. ) ;
#2484 = EDGE_CURVE ( 'NONE', #15515, #7123, #21845, .T. ) ;
#2485 = CARTESIAN_POINT ( 'NONE',  ( 7.499999999999965361, -14.00000000000003020, 9.250000000000021316 ) ) ;
#2486 = LINE ( 'NONE', #20503, #13438 ) ;
#2487 = CARTESIAN_POINT ( 'NONE',  ( 66.26395429947835680, -4.500000000000003553, -6.500000000000081712 ) ) ;
#2488 = DIRECTION ( 'NONE',  ( -0.6666666666666649643, -4.683861624749726065E-31, -0.7453559924999314523 ) ) ;
#2489 = ORIENTED_EDGE ( 'NONE', *, *, #5645, .F. ) ;
#2490 = TOROIDAL_SURFACE ( 'NONE', #8901, 6.500000000000000888, 0.5000000000000000000 ) ;
#2492 = EDGE_LOOP ( 'NONE', ( #35, #15607, #5667, #17989 ) ) ;
#2491 = ORIENTED_EDGE ( 'NONE', *, *, #14431, .F. ) ;
#2493 = UNCERTAINTY_MEASURE_WITH_UNIT (LENGTH_MEASURE( 1.000000000000000082E-05 ), #11423, 'distance_accuracy_value', 'NONE');
#2494 = ADVANCED_FACE ( 'NONE', ( #13247 ), #6075, .F. ) ;
#2495 = EDGE_LOOP ( 'NONE', ( #7906, #19985, #5114, #4922 ) ) ;
#2496 = ORIENTED_EDGE ( 'NONE', *, *, #11857, .F. ) ;
#2499 = ORIENTED_EDGE ( 'NONE', *, *, #15948, .F. ) ;
#2498 = EDGE_CURVE ( 'NONE', #9471, #23120, #9205, .T. ) ;
#2497 = ORIENTED_EDGE ( 'NONE', *, *, #13892, .T. ) ;
#2500 = VERTEX_POINT ( 'NONE', #2074 ) ;
#2501 = DIRECTION ( 'NONE',  ( -2.775557561562883647E-17, 3.406761633869147840E-16, -1.000000000000000000 ) ) ;
#2502 = DIRECTION ( 'NONE',  ( 1.000000000000000000, 1.479114197289388027E-30, -2.013525853228518840E-32 ) ) ;
#2503 = EDGE_LOOP ( 'NONE', ( #9497, #6072, #10283, #14107 ) ) ;
#2504 = TOROIDAL_SURFACE ( 'NONE', #11151, 1.300000000000000711, 0.5000000000000000000 ) ;
#2505 = DIRECTION ( 'NONE',  ( 0.000000000000000000, 1.000000000000000000, 0.000000000000000000 ) ) ;
#2506 = CARTESIAN_POINT ( 'NONE',  ( -6.495190528383341544, 4.999999999999920952, 3.750000000000017319 ) ) ;
#2507 = DIRECTION ( 'NONE',  ( 1.000000000000000000, 4.440892098500626162E-16, -5.551115123125782702E-16 ) ) ;
#2508 = CARTESIAN_POINT ( 'NONE',  ( 5.600000000000000533, 0.000000000000000000, -3.469446951953614189E-15 ) ) ;
#2509 = VECTOR ( 'NONE', #13919, 1000.000000000000000 ) ;
#2510 = CARTESIAN_POINT ( 'NONE',  ( 2.499999999999960476, 4.500000000000017764, -18.75000000000002132 ) ) ;
#2511 = FACE_OUTER_BOUND ( 'NONE', #12858, .T. ) ;
#2512 = CARTESIAN_POINT ( 'NONE',  ( 4.180231680468780020, -2.085385483809547136, 3.570466434508575926 ) ) ;
#2513 = AXIS2_PLACEMENT_3D ( 'NONE', #14721, #9085, #20142 ) ;
#2514 = CYLINDRICAL_SURFACE ( 'NONE', #17562, 2.100000000000011635 ) ;
#2515 = CARTESIAN_POINT ( 'NONE',  ( 0.2500000000000036637, 2.000000000000001776, -17.00000000000000711 ) ) ;
#2516 = DIRECTION ( 'NONE',  ( -8.438582421954109416E-32, 0.000000000000000000, -1.000000000000000000 ) ) ;
#2517 = DIRECTION ( 'NONE',  ( 0.1556420233463076119, 0.000000000000000000, 0.9878135252003121813 ) ) ;
#2518 = ORIENTED_EDGE ( 'NONE', *, *, #1466, .T. ) ;
#2519 = UNCERTAINTY_MEASURE_WITH_UNIT (LENGTH_MEASURE( 1.000000000000000082E-05 ), #17091, 'distance_accuracy_value', 'NONE');
#2521 = ORIENTED_EDGE ( 'NONE', *, *, #13323, .T. ) ;
#2520 = ORIENTED_EDGE ( 'NONE', *, *, #16854, .F. ) ;
#2522 = EDGE_CURVE ( 'NONE', #11952, #11922, #5989, .T. ) ;
#2523 = AXIS2_PLACEMENT_3D ( 'NONE', #1490, #14193, #6906 ) ;
#2524 = ORIENTED_EDGE ( 'NONE', *, *, #1467, .T. ) ;
#2525 = CIRCLE ( 'NONE', #7048, 0.4999999999999984457 ) ;
#2526 = VERTEX_POINT ( 'NONE', #9485 ) ;
#2527 = ADVANCED_FACE ( 'NONE', ( #9725 ), #320, .T. ) ;
#2528 = EDGE_LOOP ( 'NONE', ( #5964, #777, #21753, #424, #12855 ) ) ;
#2529 = ADVANCED_FACE ( 'NONE', ( #18654 ), #11011, .T. ) ;
#2530 = EDGE_LOOP ( 'NONE', ( #21268, #3944, #20296, #7541 ) ) ;
#2531 = DIRECTION ( 'NONE',  ( 0.6819983600624981435, -0.7313537016191709039, 0.000000000000000000 ) ) ;
#2532 = CARTESIAN_POINT ( 'NONE',  ( -7.499999999999992895, -8.000000000000003553, 11.74999999999999645 ) ) ;
#2533 = ORIENTED_EDGE ( 'NONE', *, *, #15752, .F. ) ;
#2534 = AXIS2_PLACEMENT_3D ( 'NONE', #13114, #9701, #5840 ) ;
#2535 = CARTESIAN_POINT ( 'NONE',  ( 4.175326769692852658, -4.121399112977865542, -6.938946365301216616E-15 ) ) ;
#2536 = LINE ( 'NONE', #7952, #7258 ) ;
#2537 = DIRECTION ( 'NONE',  ( -0.8122328620674128530, 0.000000000000000000, -0.5833333333333344806 ) ) ;
#2538 = AXIS2_PLACEMENT_3D ( 'NONE', #2743, #18987, #23079 ) ;
#2539 = CYLINDRICAL_SURFACE ( 'NONE', #15084, 4.750000000000013323 ) ;
#2540 = DIRECTION ( 'NONE',  ( -0.5150787536377141596, 0.000000000000000000, -0.8571428571428563181 ) ) ;
#2541 = VECTOR ( 'NONE', #5687, 1000.000000000000000 ) ;
#2542 = CARTESIAN_POINT ( 'NONE',  ( -7.490313984279750592, -13.85571552873294188, 7.566633644154753924 ) ) ;
#2543 = DIRECTION ( 'NONE',  ( -1.000000000000000000, 1.389842848855773367E-62, -2.013525853228507892E-32 ) ) ;
#2544 = LINE ( 'NONE', #9732, #1655 ) ;
#2545 = CIRCLE ( 'NONE', #6686, 1.300000000000009592 ) ;
#2546 = CARTESIAN_POINT ( 'NONE',  ( 37.73505106183116453, 7.752354164078167471E-12, -10.73505106183309543 ) ) ;
#2547 = VECTOR ( 'NONE', #4832, 1000.000000000000000 ) ;
#2548 =( NAMED_UNIT ( * ) SI_UNIT ( $, .STERADIAN. ) SOLID_ANGLE_UNIT ( ) );
#2549 = CARTESIAN_POINT ( 'NONE',  ( 25.60000000000000142, 0.000000000000000000, -6.938893903907228378E-15 ) ) ;
#2550 = CARTESIAN_POINT ( 'NONE',  ( 33.59619407800441593, 21.59619407671642222, -26.00000000000000000 ) ) ;
#2551 = AXIS2_PLACEMENT_3D ( 'NONE', #15228, #8069, #16879 ) ;
#2552 = ORIENTED_EDGE ( 'NONE', *, *, #13276, .T. ) ;
#2553 = ORIENTED_EDGE ( 'NONE', *, *, #1879, .T. ) ;
#2554 = ORIENTED_EDGE ( 'NONE', *, *, #22201, .F. ) ;
#2555 = ORIENTED_EDGE ( 'NONE', *, *, #17567, .F. ) ;
#2556 = ORIENTED_EDGE ( 'NONE', *, *, #20753, .F. ) ;
#2557 = PRESENTATION_LAYER_ASSIGNMENT (  '', '', ( #1083 ) ) ;
#2558 = FACE_OUTER_BOUND ( 'NONE', #8206, .T. ) ;
#2559 = DIRECTION ( 'NONE',  ( -2.168404344971017743E-16, 1.000000000000000000, 7.722382221513089478E-47 ) ) ;
#2560 = VERTEX_POINT ( 'NONE', #13020 ) ;
#2561 = CIRCLE ( 'NONE', #20610, 3.300000000000020250 ) ;
#2562 = CARTESIAN_POINT ( 'NONE',  ( -95.70000000000059970, -2.700000000000119194, -2.000000000000029310 ) ) ;
#2563 = DIRECTION ( 'NONE',  ( 1.550910762415566494E-16, 1.000000000000000000, -8.135128085091684243E-31 ) ) ;
#2564 = CARTESIAN_POINT ( 'NONE',  ( 1.387778780781445676E-14, 4.618802153517020059, -5.600000000000000533 ) ) ;
#2565 = CIRCLE ( 'NONE', #15708, 10.00000000000006395 ) ;
#2566 = CIRCLE ( 'NONE', #7831, 0.4999999999999993894 ) ;
#2567 = DIRECTION ( 'NONE',  ( -1.000000000000000000, -2.699383410053119644E-30, -3.330669073875432643E-16 ) ) ;
#2568 = CIRCLE ( 'NONE', #7466, 2.999999999999999112 ) ;
#2569 = DIRECTION ( 'NONE',  ( -1.333893503340774882E-15, -2.778352770573747380E-17, -1.000000000000000000 ) ) ;
#2570 = DIRECTION ( 'NONE',  ( 1.000000000000000000, -4.190823558986610327E-31, 1.733449886265890494E-32 ) ) ;
#2571 = ADVANCED_FACE ( 'NONE', ( #7722 ), #7604, .F. ) ;
#2572 = DIRECTION ( 'NONE',  ( -3.032184104443272185E-30, -1.000000000000000000, 7.395570986447005381E-32 ) ) ;
#2573 = DIRECTION ( 'NONE',  ( -2.013525853228507892E-32, -6.902532920683810383E-31, 1.000000000000000000 ) ) ;
#2574 = CARTESIAN_POINT ( 'NONE',  ( -64.00000000000038369, -2.700000000000091216, -2.000000000000029310 ) ) ;
#2575 = DIRECTION ( 'NONE',  ( 4.190823558986625216E-31, -1.000000000000000000, 4.190823558986625216E-31 ) ) ;
#2576 = CYLINDRICAL_SURFACE ( 'NONE', #6610, 0.5000000000000038858 ) ;
#2577 =( GEOMETRIC_REPRESENTATION_CONTEXT ( 3 ) GLOBAL_UNCERTAINTY_ASSIGNED_CONTEXT ( ( #10247 ) ) GLOBAL_UNIT_ASSIGNED_CONTEXT ( ( #7825, #14880, #7366 ) ) REPRESENTATION_CONTEXT ( 'NONE', 'WORKASPACE' ) );
#2578 = CARTESIAN_POINT ( 'NONE',  ( 4.132952817037863547, 2.031684012687259955, -3.518979934899751694 ) ) ;
#2579 = ORIENTED_EDGE ( 'NONE', *, *, #4422, .T. ) ;
#2580 = AXIS2_PLACEMENT_3D ( 'NONE', #9270, #9616, #22204 ) ;
#2581 = AXIS2_PLACEMENT_3D ( 'NONE', #11941, #4662, #22426 ) ;
#2582 = CIRCLE ( 'NONE', #19501, 4.000000000000045297 ) ;
#2583 = ORIENTED_EDGE ( 'NONE', *, *, #2663, .F. ) ;
#2585 = ORIENTED_EDGE ( 'NONE', *, *, #2797, .F. ) ;
#2584 = ORIENTED_EDGE ( 'NONE', *, *, #1979, .T. ) ;
#2586 = CARTESIAN_POINT ( 'NONE',  ( 2.775557561562891351E-14, 2.499999999999998668, -6.499999999999950262 ) ) ;
#2587 = DIRECTION ( 'NONE',  ( -1.550910762415566494E-16, -1.000000000000000000, 8.135128085091684243E-31 ) ) ;
#2588 = FACE_OUTER_BOUND ( 'NONE', #14280, .T. ) ;
#2589 = ORIENTED_EDGE ( 'NONE', *, *, #13484, .F. ) ;
#2590 = LINE ( 'NONE', #9772, #8971 ) ;
#2591 = DIRECTION ( 'NONE',  ( -1.000000000000000000, -1.387778780781438734E-14, -1.404432126150815135E-14 ) ) ;
#2592 = DIRECTION ( 'NONE',  ( 1.000000000000000000, 2.220446049250313081E-16, -3.656342123407315983E-48 ) ) ;
#2593 = EDGE_CURVE ( 'NONE', #16059, #19782, #2582, .T. ) ;
#2594 = CARTESIAN_POINT ( 'NONE',  ( 30.60000000000000142, 2.775557561562891351E-14, 2.054999999999978844 ) ) ;
#2595 = AXIS2_PLACEMENT_3D ( 'NONE', #10540, #18195, #9242 ) ;
#2596 = DIRECTION ( 'NONE',  ( 1.000000000000000000, 0.000000000000000000, 0.000000000000000000 ) ) ;
#2597 = AXIS2_PLACEMENT_3D ( 'NONE', #11130, #14661, #20203 ) ;
#2598 = DIRECTION ( 'NONE',  ( 1.000000000000000000, 1.910522504832140594E-31, -5.551115123125818447E-17 ) ) ;
#2599 = SURFACE_SIDE_STYLE ('',( #18380 ) ) ;
#2600 = DIRECTION ( 'NONE',  ( 5.551115123561405253E-17, 1.000000000000000000, 2.256980353643891447E-27 ) ) ;
#2601 = EDGE_CURVE ( 'NONE', #15092, #2139, #8615, .T. ) ;
#2602 = DIRECTION ( 'NONE',  ( -0.7071067811865530128, -8.067112339249838682E-32, 0.7071067811865421326 ) ) ;
#2603 = CARTESIAN_POINT ( 'NONE',  ( -95.20000000000065654, 6.938893903907228378E-15, 1.000000000000042633 ) ) ;
#2605 = ADVANCED_FACE ( 'NONE', ( #14780 ), #18763, .T. ) ;
#2604 = CIRCLE ( 'NONE', #19520, 9.500000000000056843 ) ;
#2606 = CARTESIAN_POINT ( 'NONE',  ( 8.660254037844413944, 4.689110867544616035, 2.775557561562891351E-14 ) ) ;
#2607 = CARTESIAN_POINT ( 'NONE',  ( -95.20000000000065654, 3.200000000000015277, 1.000000000000042633 ) ) ;
#2608 = EDGE_CURVE ( 'NONE', #3717, #14311, #20313, .T. ) ;
#2609 = MECHANICAL_DESIGN_GEOMETRIC_PRESENTATION_REPRESENTATION (  '', ( #16115 ), #19899 ) ;
#2610 = ORIENTED_EDGE ( 'NONE', *, *, #15468, .F. ) ;
#2612 = ORIENTED_EDGE ( 'NONE', *, *, #20821, .T. ) ;
#2611 = ORIENTED_EDGE ( 'NONE', *, *, #1787, .F. ) ;
#2613 = ORIENTED_EDGE ( 'NONE', *, *, #6350, .F. ) ;
#2614 = ORIENTED_EDGE ( 'NONE', *, *, #1237, .T. ) ;
#2615 =( BOUNDED_CURVE ( )  B_SPLINE_CURVE ( 3, ( #11377, #12923, #10910, #452 ),
 .UNSPECIFIED., .F., .F. ) 
 B_SPLINE_CURVE_WITH_KNOTS ( ( 4, 4 ),
 ( 1.570796326794896558, 2.617993877991555252 ),
 .UNSPECIFIED. ) 
 CURVE ( )  GEOMETRIC_REPRESENTATION_ITEM ( )  RATIONAL_B_SPLINE_CURVE ( ( 1.000000000000000000, 0.9106836025229487763, 0.9106836025229487763, 1.000000000000000000 ) ) 
 REPRESENTATION_ITEM ( '' )  );
#2617 = ORIENTED_EDGE ( 'NONE', *, *, #7108, .F. ) ;
#2616 = ORIENTED_EDGE ( 'NONE', *, *, #2459, .T. ) ;
#2618 = ORIENTED_EDGE ( 'NONE', *, *, #12520, .F. ) ;
#2619 = DIRECTION ( 'NONE',  ( -1.000000000000000000, -4.440892098500626162E-16, 5.551115123125782702E-16 ) ) ;
#2620 = EDGE_CURVE ( 'NONE', #5493, #22681, #14628, .T. ) ;
#2621 = CARTESIAN_POINT ( 'NONE',  ( 119.5756419024614559, 2.499999999999974243, -5.999999999999963585 ) ) ;
#2622 = ORIENTED_EDGE ( 'NONE', *, *, #6541, .T. ) ;
#2623 = EDGE_CURVE ( 'NONE', #3689, #12152, #5622, .T. ) ;
#2624 = SURFACE_STYLE_USAGE ( .BOTH. , #18851 ) ;
#2625 = AXIS2_PLACEMENT_3D ( 'NONE', #11795, #8154, #20750 ) ;
#2626 = CARTESIAN_POINT ( 'NONE',  ( -91.14322581977729953, 6.938893903907228378E-15, 6.823838874241844543 ) ) ;
#2627 = DIRECTION ( 'NONE',  ( -1.000000000000000000, -2.220446049250301001E-16, 0.000000000000000000 ) ) ;
#2628 = APPLICATION_CONTEXT ( 'automotive_design' ) ;
#2629 = CARTESIAN_POINT ( 'NONE',  ( -50.65685424949267457, 7.200000000000018829, -7.500000000000034639 ) ) ;
#2630 = PRESENTATION_LAYER_ASSIGNMENT (  '', '', ( #4867 ) ) ;
#2631 = CARTESIAN_POINT ( 'NONE',  ( 42.00000000000014921, 2.999999999999999112, -15.00000000000001421 ) ) ;
#2632 = DIRECTION ( 'NONE',  ( -1.000000000000000000, 0.000000000000000000, 1.613696256722611405E-16 ) ) ;
#2633 = CARTESIAN_POINT ( 'NONE',  ( 7.725871784772784245, -1.814340584914947430, 8.100883686804943196 ) ) ;
#2634 = CARTESIAN_POINT ( 'NONE',  ( 3.974183935050594307, -0.7239581970533454092, 3.565826011443202770 ) ) ;
#2635 = EDGE_CURVE ( 'NONE', #11002, #8317, #15741, .T. ) ;
#2636 = DIRECTION ( 'NONE',  ( 1.000000000000000000, 2.168404344970992105E-16, -5.204170427930381051E-15 ) ) ;
#2637 = ADVANCED_FACE ( 'NONE', ( #16988 ), #8429, .F. ) ;
#2638 = FACE_OUTER_BOUND ( 'NONE', #5699, .T. ) ;
#2639 = CYLINDRICAL_SURFACE ( 'NONE', #9314, 7.000000000000075495 ) ;
#2640 = EDGE_CURVE ( 'NONE', #23176, #18021, #6653, .T. ) ;
#2641 = ORIENTED_EDGE ( 'NONE', *, *, #10946, .T. ) ;
#2642 = VECTOR ( 'NONE', #1442, 1000.000000000000000 ) ;
#2644 = VERTEX_POINT ( 'NONE', #22776 ) ;
#2643 = EDGE_LOOP ( 'NONE', ( #9016, #7011, #20838, #17686 ) ) ;
#2645 = EDGE_LOOP ( 'NONE', ( #17463, #13928, #18590 ) ) ;
#2646 = ORIENTED_EDGE ( 'NONE', *, *, #3704, .F. ) ;
#2647 = ORIENTED_EDGE ( 'NONE', *, *, #17863, .T. ) ;
#2648 = ORIENTED_EDGE ( 'NONE', *, *, #9543, .T. ) ;
#2649 = LINE ( 'NONE', #16753, #21587 ) ;
#2650 = ADVANCED_FACE ( 'NONE', ( #4411 ), #21010, .T. ) ;
#2651 = DIRECTION ( 'NONE',  ( -1.000000000000000000, -0.000000000000000000, 1.613696256722611405E-16 ) ) ;
#2652 = VERTEX_POINT ( 'NONE', #15466 ) ;
#2653 = CYLINDRICAL_SURFACE ( 'NONE', #7597, 0.4999999999999987232 ) ;
#2654 = CARTESIAN_POINT ( 'NONE',  ( 4.158413352280808439, 2.044871626972768919, 3.541821552872997714 ) ) ;
#2655 = CARTESIAN_POINT ( 'NONE',  ( 0.6666666666666630769, 4.233901974057274309, -3.300726591567085144 ) ) ;
#2656 = AXIS2_PLACEMENT_3D ( 'NONE', #6369, #13310, #14944 ) ;
#2657 = CARTESIAN_POINT ( 'NONE',  ( -47.82842712474658242, 4.371572875253824542, -7.500000000000007105 ) ) ;
#2658 = EDGE_CURVE ( 'NONE', #13530, #16493, #11950, .T. ) ;
#2659 = CARTESIAN_POINT ( 'NONE',  ( 119.5756419024615411, -7.000000000000006217, 6.000000000000095923 ) ) ;
#2660 = CARTESIAN_POINT ( 'NONE',  ( -7.876571740167121582, -13.80606002021568735, 7.785394814391164431 ) ) ;
#2661 = FACE_BOUND ( 'NONE', #20938, .T. ) ;
#2662 = DIRECTION ( 'NONE',  ( 1.066786462891689527E-26, 6.656013887802287108E-31, 1.000000000000000000 ) ) ;
#2663 = EDGE_CURVE ( 'NONE', #9669, #7684, #12697, .T. ) ;
#2664 = CARTESIAN_POINT ( 'NONE',  ( 6.000000000291855429, 2.999999999003851503, 0.000000000000000000 ) ) ;
#2665 = EDGE_LOOP ( 'NONE', ( #9213, #15572, #3033, #14858 ) ) ;
#2666 = FACE_OUTER_BOUND ( 'NONE', #8055, .T. ) ;
#2667 = CARTESIAN_POINT ( 'NONE',  ( 3.000000000000002665, 0.000000000000000000, 0.000000000000000000 ) ) ;
#2668 = ORIENTED_EDGE ( 'NONE', *, *, #7782, .T. ) ;
#2669 = ORIENTED_EDGE ( 'NONE', *, *, #2077, .T. ) ;
#2670 = CONICAL_SURFACE ( 'NONE', #3064, 4.750000000000000000, 1.047197551196600074 ) ;
#2671 = ORIENTED_EDGE ( 'NONE', *, *, #17854, .T. ) ;
#2672 = ORIENTED_EDGE ( 'NONE', *, *, #557, .T. ) ;
#2673 = DIRECTION ( 'NONE',  ( -0.7313537016191730133, 0.6819983600624957010, -5.924440990721418971E-17 ) ) ;
#2674 = CARTESIAN_POINT ( 'NONE',  ( -42.54314575050782565, -7.500000000000038192, -8.000000000000007105 ) ) ;
#2675 = EDGE_LOOP ( 'NONE', ( #8873, #5208, #5490, #18056 ) ) ;
#2676 = DIRECTION ( 'NONE',  ( -1.000000000000000000, 0.000000000000000000, -1.066687855278535322E-26 ) ) ;
#2677 = LINE ( 'NONE', #11614, #7400 ) ;
#2678 = DIRECTION ( 'NONE',  ( -9.693522803355793065E-26, 5.963788443470849249E-28, 1.000000000000000000 ) ) ;
#2679 = CARTESIAN_POINT ( 'NONE',  ( -6.975867733769219647, 36.00005661733510465, -18.50635935043928981 ) ) ;
#2680 = DIRECTION ( 'NONE',  ( -2.013525853228507892E-32, -6.902532920683810383E-31, 1.000000000000000000 ) ) ;
#2681 = CARTESIAN_POINT ( 'NONE',  ( 2.775557561562891351E-14, 8.500000000000003553, -6.499999999999950262 ) ) ;
#2682 = EDGE_CURVE ( 'NONE', #8464, #9707, #10899, .T. ) ;
#2683 = CARTESIAN_POINT ( 'NONE',  ( -7.500000000000020428, -1.223704156646857388, 9.030675447288954771 ) ) ;
#2684 = FACE_OUTER_BOUND ( 'NONE', #22293, .T. ) ;
#2685 = CARTESIAN_POINT ( 'NONE',  ( 30.00000000029184832, 2.999999999003851503, -5.999999999999998224 ) ) ;
#2686 = CIRCLE ( 'NONE', #3811, 0.5000000000000028866 ) ;
#2687 = AXIS2_PLACEMENT_3D ( 'NONE', #8853, #14682, #16009 ) ;
#2688 = CARTESIAN_POINT ( 'NONE',  ( 80.49335071782266482, -7.708908342713566064, -6.500000000000047073 ) ) ;
#2689 = LINE ( 'NONE', #20583, #5218 ) ;
#2690 = DIRECTION ( 'NONE',  ( -1.000000000000000000, 1.387778780781435420E-14, 9.144641450333394555E-31 ) ) ;
#2691 = ADVANCED_FACE ( 'NONE', ( #17109 ), #790, .F. ) ;
#2692 = DIRECTION ( 'NONE',  ( 1.000000000000000000, 0.000000000000000000, 1.581383788144386089E-16 ) ) ;
#2693 = ORIENTED_EDGE ( 'NONE', *, *, #12821, .F. ) ;
#2695 = ORIENTED_EDGE ( 'NONE', *, *, #1025, .F. ) ;
#2694 = VERTEX_POINT ( 'NONE', #20789 ) ;
#2696 = CIRCLE ( 'NONE', #9847, 0.5000000000000004441 ) ;
#2697 = AXIS2_PLACEMENT_3D ( 'NONE', #18422, #11347, #18538 ) ;
#2698 = DIRECTION ( 'NONE',  ( 0.000000000000000000, 0.000000000000000000, -1.000000000000000000 ) ) ;
#2699 = CARTESIAN_POINT ( 'NONE',  ( 30.00000000029184832, 2.999999999003851503, -3.449999999999999289 ) ) ;
#2700 = DIRECTION ( 'NONE',  ( -1.000000000000000000, 7.100545512326564696E-57, 1.066786462891689527E-26 ) ) ;
#2701 = EDGE_LOOP ( 'NONE', ( #12986, #7252, #2247, #12420 ) ) ;
#2702 = CARTESIAN_POINT ( 'NONE',  ( 4.093692494532776394, 4.043567292011502445, 6.937578715282024528E-15 ) ) ;
#2703 = FACE_OUTER_BOUND ( 'NONE', #18173, .T. ) ;
#2704 = DIRECTION ( 'NONE',  ( -0.6666666666666649643, -2.585973076299232148E-15, -0.7453559924999314523 ) ) ;
#2705 = FACE_OUTER_BOUND ( 'NONE', #15944, .T. ) ;
#2706 = FACE_OUTER_BOUND ( 'NONE', #18363, .T. ) ;
#2707 = CIRCLE ( 'NONE', #14736, 5.000000000000000888 ) ;
#2708 = CYLINDRICAL_SURFACE ( 'NONE', #11715, 9.000000000000031974 ) ;
#2709 = LINE ( 'NONE', #4826, #17444 ) ;
#2710 = DIRECTION ( 'NONE',  ( -5.861751848416504610E-18, 0.9863939238321435266, -0.1643989873053580686 ) ) ;
#2711 = DIRECTION ( 'NONE',  ( 2.013525853228508439E-32, 6.779273404243028164E-31, -1.000000000000000000 ) ) ;
#2712 = SURFACE_STYLE_USAGE ( .BOTH. , #15184 ) ;
#2713 = CIRCLE ( 'NONE', #17752, 2.999999999999999112 ) ;
#2714 = DIRECTION ( 'NONE',  ( 0.000000000000000000, 0.000000000000000000, 1.000000000000000000 ) ) ;
#2716 = CIRCLE ( 'NONE', #19635, 2.500000000000015987 ) ;
#2715 = CARTESIAN_POINT ( 'NONE',  ( -12.85000000000001386, -12.00000000000006928, 4.163336342344337027E-14 ) ) ;
#2717 = CIRCLE ( 'NONE', #5358, 6.000000000000047962 ) ;
#2718 = VERTEX_POINT ( 'NONE', #22660 ) ;
#2719 = CONICAL_SURFACE ( 'NONE', #16247, 2.055000000000002380, 0.7853981633974400633 ) ;
#2720 = PRODUCT_RELATED_PRODUCT_CATEGORY ( 'part', '', ( #6869 ) ) ;
#2722 = ORIENTED_EDGE ( 'NONE', *, *, #7766, .T. ) ;
#2721 = ORIENTED_EDGE ( 'NONE', *, *, #5530, .F. ) ;
#2723 = ADVANCED_FACE ( 'NONE', ( #13719 ), #20984, .F. ) ;
#2724 = ORIENTED_EDGE ( 'NONE', *, *, #14425, .F. ) ;
#2726 = ORIENTED_EDGE ( 'NONE', *, *, #22779, .F. ) ;
#2725 = VERTEX_POINT ( 'NONE', #15586 ) ;
#2727 = AXIS2_PLACEMENT_3D ( 'NONE', #13546, #2957, #12109 ) ;
#2728 = ORIENTED_EDGE ( 'NONE', *, *, #8529, .T. ) ;
#2729 = DIRECTION ( 'NONE',  ( 1.000000000000000000, 2.168404344971017743E-16, -1.780660105995169760E-30 ) ) ;
#2730 = DIRECTION ( 'NONE',  ( -7.395570986446975166E-31, -3.382522293539642681E-32, -1.000000000000000000 ) ) ;
#2731 = ORIENTED_EDGE ( 'NONE', *, *, #16144, .F. ) ;
#2732 = ADVANCED_FACE ( 'NONE', ( #19014 ), #13487, .F. ) ;
#2733 = AXIS2_PLACEMENT_3D ( 'NONE', #18854, #2739, #4616 ) ;
#2734 = DIRECTION ( 'NONE',  ( -1.000000000000000000, 1.847414967615758933E-47, -3.885780586188017323E-16 ) ) ;
#2735 = B_SPLINE_CURVE_WITH_KNOTS ( 'NONE', 3,
 ( #9115, #2163, #16388, #9350, #16616 ),
 .UNSPECIFIED., .F., .F.,
 ( 4, 1, 4 ),
 ( 0.000000000000000000, 0.002020725942163690073, 0.004041451884327380145 ),
 .UNSPECIFIED. ) ;
#2736 = AXIS2_PLACEMENT_3D ( 'NONE', #13824, #10172, #12398 ) ;
#2737 = DIRECTION ( 'NONE',  ( 0.000000000000000000, 0.000000000000000000, -1.000000000000000000 ) ) ;
#2738 = CIRCLE ( 'NONE', #15498, 2.500000000000000444 ) ;
#2739 = DIRECTION ( 'NONE',  ( -1.000000000000000000, -3.254448077276381206E-32, -1.066788928082016908E-26 ) ) ;
#2740 = VECTOR ( 'NONE', #16468, 1000.000000000000000 ) ;
#2741 = CARTESIAN_POINT ( 'NONE',  ( 0.2500000000000036637, 1.387778780781445676E-14, -19.00000000000001066 ) ) ;
#2742 = LINE ( 'NONE', #2510, #17374 ) ;
#2743 = CARTESIAN_POINT ( 'NONE',  ( 108.2426266706970637, -13.52760560296348302, 6.500000000000019540 ) ) ;
#2744 = CARTESIAN_POINT ( 'NONE',  ( 3.974183935050618732, -0.7239581970533588429, 3.565826011443267163 ) ) ;
#2745 = EDGE_CURVE ( 'NONE', #2319, #5235, #5570, .T. ) ;
#2746 = FACE_OUTER_BOUND ( 'NONE', #13879, .T. ) ;
#2747 = DIRECTION ( 'NONE',  ( 7.860214984770699307E-18, -1.409037165336591006E-16, -1.000000000000000000 ) ) ;
#2748 = DIRECTION ( 'NONE',  ( 2.013525853228507892E-32, 6.902532920683810383E-31, -1.000000000000000000 ) ) ;
#2749 = CARTESIAN_POINT ( 'NONE',  ( 6.000000000291855429, -9.961476088449217059E-10, -8.549999999999998934 ) ) ;
#2750 = CARTESIAN_POINT ( 'NONE',  ( 4.030859730899970295, -1.403482646611178053, -3.500000000000007105 ) ) ;
#2751 = ORIENTED_EDGE ( 'NONE', *, *, #8398, .F. ) ;
#2752 = PRODUCT_DEFINITION_CONTEXT ( 'detailed design', #16293, 'design' ) ;
#2753 = EDGE_CURVE ( 'NONE', #20007, #4400, #20598, .T. ) ;
#2754 = VECTOR ( 'NONE', #7282, 1000.000000000000114 ) ;
#2755 = AXIS2_PLACEMENT_3D ( 'NONE', #8649, #17468, #6768 ) ;
#2757 = ORIENTED_EDGE ( 'NONE', *, *, #4488, .F. ) ;
#2756 = EDGE_LOOP ( 'NONE', ( #17452, #7889, #14961, #19393 ) ) ;
#2758 = AXIS2_PLACEMENT_3D ( 'NONE', #16955, #13884, #15520 ) ;
#2759 = AXIS2_PLACEMENT_3D ( 'NONE', #22819, #3293, #7175 ) ;
#2761 = EDGE_CURVE ( 'NONE', #9641, #18414, #22476, .T. ) ;
#2760 = AXIS2_PLACEMENT_3D ( 'NONE', #16922, #2698, #8347 ) ;
#2762 = ORIENTED_EDGE ( 'NONE', *, *, #1632, .T. ) ;
#2763 = TOROIDAL_SURFACE ( 'NONE', #5779, 2.250000000000000444, 0.2500000000000000000 ) ;
#2764 = ORIENTED_EDGE ( 'NONE', *, *, #13415, .T. ) ;
#2765 = APPLICATION_CONTEXT ( 'automotive_design' ) ;
#2766 = ORIENTED_EDGE ( 'NONE', *, *, #21500, .T. ) ;
#2767 = CARTESIAN_POINT ( 'NONE',  ( 7.949747468597695210, 47.94974746730969173, -15.99999999999999289 ) ) ;
#2768 = ADVANCED_FACE ( 'NONE', ( #6428 ), #15115, .T. ) ;
#2769 = ADVANCED_FACE ( 'NONE', ( #10069 ), #13858, .T. ) ;
#2770 = DIRECTION ( 'NONE',  ( 9.121204216617949000E-31, 1.000000000000000000, -6.982962677686261977E-15 ) ) ;
#2771 = ORIENTED_EDGE ( 'NONE', *, *, #17419, .F. ) ;
#2772 = DIRECTION ( 'NONE',  ( 2.013525853228507892E-32, 6.902532920683810383E-31, -1.000000000000000000 ) ) ;
#2773 = EDGE_CURVE ( 'NONE', #11457, #2292, #3041, .T. ) ;
#2774 = DIRECTION ( 'NONE',  ( 5.423418723394450907E-31, 0.5000000000000015543, 0.8660254037844377084 ) ) ;
#2775 = AXIS2_PLACEMENT_3D ( 'NONE', #1028, #1258, #8197 ) ;
#2776 = CARTESIAN_POINT ( 'NONE',  ( 4.175572532730933872, 2.061029303918013866, 3.569807470274402483 ) ) ;
#2777 = CIRCLE ( 'NONE', #17813, 2.549999999999997158 ) ;
#2778 = CARTESIAN_POINT ( 'NONE',  ( 0.000000000000000000, 0.000000000000000000, -5.600000000000000533 ) ) ;
#2779 = LINE ( 'NONE', #12171, #21502 ) ;
#2780 = CARTESIAN_POINT ( 'NONE',  ( 4.170895651974849905, 4.109780709045216973, 2.320551093086091258E-18 ) ) ;
#2781 = CARTESIAN_POINT ( 'NONE',  ( -7.951003271401806849, -13.83829779185615294, 7.659883344695980867 ) ) ;
#2782 = PLANE ( 'NONE',  #19125 ) ;
#2783 = CARTESIAN_POINT ( 'NONE',  ( 1.040834085586084257E-14, 4.500000000000003553, 0.000000000000000000 ) ) ;
#2784 = EDGE_CURVE ( 'NONE', #13233, #18266, #3011, .T. ) ;
#2785 = CARTESIAN_POINT ( 'NONE',  ( 12.49999999999996625, 0.2500000000000002220, -9.500000000000003553 ) ) ;
#2786 = EDGE_CURVE ( 'NONE', #17843, #3270, #1821, .T. ) ;
#2787 = ORIENTED_EDGE ( 'NONE', *, *, #9230, .T. ) ;
#2788 = EDGE_CURVE ( 'NONE', #2802, #13206, #16846, .T. ) ;
#2789 = EDGE_CURVE ( 'NONE', #10026, #18942, #16089, .T. ) ;
#2790 = CARTESIAN_POINT ( 'NONE',  ( -4.113620667976075396, -1.750000000000001554, 2.374999999999986677 ) ) ;
#2791 = DIRECTION ( 'NONE',  ( 1.000000000000000000, 6.224605580259554159E-31, -2.887593071917436153E-31 ) ) ;
#2792 = ORIENTED_EDGE ( 'NONE', *, *, #16542, .T. ) ;
#2793 = VECTOR ( 'NONE', #2602, 999.9999999999998863 ) ;
#2794 = EDGE_LOOP ( 'NONE', ( #16780, #451, #4051, #2757 ) ) ;
#2795 = CIRCLE ( 'NONE', #21962, 4.750000000000000000 ) ;
#2796 = ORIENTED_EDGE ( 'NONE', *, *, #44, .T. ) ;
#2797 = EDGE_CURVE ( 'NONE', #6091, #12774, #13476, .T. ) ;
#2798 = AXIS2_PLACEMENT_3D ( 'NONE', #8527, #19461, #4990 ) ;
#2799 = ORIENTED_EDGE ( 'NONE', *, *, #9962, .F. ) ;
#2800 = DIRECTION ( 'NONE',  ( 1.000000000000000000, 4.440892098500626162E-16, -5.551115123125782702E-16 ) ) ;
#2801 = DIRECTION ( 'NONE',  ( 1.000000000000000000, -7.477632011778619108E-48, 3.885780586188017323E-16 ) ) ;
#2802 = VERTEX_POINT ( 'NONE', #14180 ) ;
#2803 = EDGE_CURVE ( 'NONE', #18939, #11087, #17601, .T. ) ;
#2804 = DIRECTION ( 'NONE',  ( -1.000000000000000000, -2.699383410053119644E-30, -3.330669073875432643E-16 ) ) ;
#2805 = DIRECTION ( 'NONE',  ( -4.190823558986626092E-31, 1.000000000000000000, 4.190823558986610327E-31 ) ) ;
#2806 = EDGE_CURVE ( 'NONE', #700, #9743, #12332, .T. ) ;
#2807 =( BOUNDED_CURVE ( )  B_SPLINE_CURVE ( 3, ( #5658, #9761, #18585, #18238 ),
 .UNSPECIFIED., .F., .T. ) 
 B_SPLINE_CURVE_WITH_KNOTS ( ( 4, 4 ),
 ( 3.665191429188058070, 4.712388980384689674 ),
 .UNSPECIFIED. ) 
 CURVE ( )  GEOMETRIC_REPRESENTATION_ITEM ( )  RATIONAL_B_SPLINE_CURVE ( ( 1.000000000000000000, 0.9106836025229534393, 0.9106836025229534393, 1.000000000000000000 ) ) 
 REPRESENTATION_ITEM ( '' )  );
#2808 = LINE ( 'NONE', #2564, #11716 ) ;
#2809 = CARTESIAN_POINT ( 'NONE',  ( -89.70000000000065654, 3.200000000000057021, -2.000000000000001776 ) ) ;
#2810 = DIRECTION ( 'NONE',  ( -0.7071067811865457964, 0.7071067811865492381, 0.000000000000000000 ) ) ;
#2811 = DIRECTION ( 'NONE',  ( 1.550910762415566494E-16, 1.000000000000000000, -8.135128085091684243E-31 ) ) ;
#2812 = CARTESIAN_POINT ( 'NONE',  ( -7.500000000000020428, -1.390227771353544473, 9.250000000000008882 ) ) ;
#2813 = DIRECTION ( 'NONE',  ( -7.860214984770699307E-18, 1.409037165336591006E-16, 1.000000000000000000 ) ) ;
#2814 = AXIS2_PLACEMENT_3D ( 'NONE', #12701, #8594, #15760 ) ;
#2815 = CARTESIAN_POINT ( 'NONE',  ( -6.999999999999992006, -7.999999999999996447, 11.74999999999999645 ) ) ;
#2816 = AXIS2_PLACEMENT_3D ( 'NONE', #19426, #3327, #12013 ) ;
#2817 = LINE ( 'NONE', #2688, #3872 ) ;
#2818 = CARTESIAN_POINT ( 'NONE',  ( 5.599999999999994316, 2.020725942163688504, 3.499999999999997780 ) ) ;
#2819 = FACE_OUTER_BOUND ( 'NONE', #1943, .T. ) ;
#2820 = LINE ( 'NONE', #22935, #20615 ) ;
#2821 = ORIENTED_EDGE ( 'NONE', *, *, #2786, .F. ) ;
#2822 = VERTEX_POINT ( 'NONE', #1587 ) ;
#2823 = EDGE_CURVE ( 'NONE', #19662, #6728, #6418, .T. ) ;
#2824 = VECTOR ( 'NONE', #8683, 1000.000000000000000 ) ;
#2826 = VERTEX_POINT ( 'NONE', #74 ) ;
#2825 = ORIENTED_EDGE ( 'NONE', *, *, #11116, .T. ) ;
#2827 = AXIS2_PLACEMENT_3D ( 'NONE', #4818, #19172, #20946 ) ;
#2828 = CARTESIAN_POINT ( 'NONE',  ( 33.94974746859769255, 21.94974746730969528, -26.50000000000000000 ) ) ;
#2829 = EDGE_CURVE ( 'NONE', #6497, #19367, #17467, .T. ) ;
#2830 = CARTESIAN_POINT ( 'NONE',  ( 0.000000000000000000, 1.750000000000001554, 0.000000000000000000 ) ) ;
#2831 = CARTESIAN_POINT ( 'NONE',  ( 22.49999999999999645, 4.250000000000031974, -1.499999999999997780 ) ) ;
#2832 = VERTEX_POINT ( 'NONE', #17696 ) ;
#2833 = DIRECTION ( 'NONE',  ( 8.438582421954109416E-32, 0.000000000000000000, 1.000000000000000000 ) ) ;
#2834 = CARTESIAN_POINT ( 'NONE',  ( -42.54314575050793934, 7.999999999999992895, -7.500000000000062172 ) ) ;
#2835 = CARTESIAN_POINT ( 'NONE',  ( 2.000000000000029310, 3.464101615137740175, -5.600000000000000533 ) ) ;
#2836 = CARTESIAN_POINT ( 'NONE',  ( 4.050823680195218657, -2.400527758044904036, -2.978030508226148676 ) ) ;
#2837 = CARTESIAN_POINT ( 'NONE',  ( -6.245004513516505540E-14, -4.862606272033144883, -3.745885042887461935 ) ) ;
#2838 = CARTESIAN_POINT ( 'NONE',  ( 0.02993401039710850628, 3.373851915354574516, 1.156317065392207688 ) ) ;
#2839 = CARTESIAN_POINT ( 'NONE',  ( 3.000000000291852764, 42.99999999900385461, -26.00000000000000000 ) ) ;
#2840 = LINE ( 'NONE', #3198, #19094 ) ;
#2841 = FACE_OUTER_BOUND ( 'NONE', #18394, .T. ) ;
#2842 = DIRECTION ( 'NONE',  ( -1.000000000000000000, 1.626303258728243832E-16, -4.409088834774349725E-15 ) ) ;
#2843 = CARTESIAN_POINT ( 'NONE',  ( 2.775557561562891351E-14, 2.499999999999998668, -0.4999999999999865663 ) ) ;
#2844 = DIRECTION ( 'NONE',  ( 0.000000000000000000, 0.000000000000000000, 1.000000000000000000 ) ) ;
#2845 = ORIENTED_EDGE ( 'NONE', *, *, #6203, .F. ) ;
#2846 = AXIS2_PLACEMENT_3D ( 'NONE', #3096, #8277, #20868 ) ;
#2847 = DIRECTION ( 'NONE',  ( 1.000000000000000000, 1.151551076716827993E-12, 0.000000000000000000 ) ) ;
#2849 = ORIENTED_EDGE ( 'NONE', *, *, #7969, .F. ) ;
#2848 = VERTEX_POINT ( 'NONE', #5119 ) ;
#2850 = ORIENTED_EDGE ( 'NONE', *, *, #8237, .F. ) ;
#2852 = ORIENTED_EDGE ( 'NONE', *, *, #15065, .T. ) ;
#2851 = ORIENTED_EDGE ( 'NONE', *, *, #2077, .F. ) ;
#2853 = EDGE_LOOP ( 'NONE', ( #19452, #5309, #11785, #6845 ) ) ;
#2854 = CARTESIAN_POINT ( 'NONE',  ( -6.959810536856695151, 36.00015702695179698, -18.51059057611807646 ) ) ;
#2855 = DIRECTION ( 'NONE',  ( -0.7313537016191773432, 0.6819983600624913711, 1.628001950178159721E-16 ) ) ;
#2856 = DIRECTION ( 'NONE',  ( 1.000000000000000000, -4.437342591868175641E-31, 3.330669073875457788E-16 ) ) ;
#2857 = CARTESIAN_POINT ( 'NONE',  ( 25.60000000000000142, 0.000000000000000000, -6.938893903907228378E-15 ) ) ;
#2858 = CARTESIAN_POINT ( 'NONE',  ( 0.000000000000000000, 0.000000000000000000, 0.000000000000000000 ) ) ;
#2859 = CARTESIAN_POINT ( 'NONE',  ( -2.500000000000000444, 3.061616997868383634E-16, 3.415236843329338967E-15 ) ) ;
#2860 = CARTESIAN_POINT ( 'NONE',  ( -95.20000000000058549, -2.700000000000119194, 8.000000000000035527 ) ) ;
#2861 = AXIS2_PLACEMENT_3D ( 'NONE', #21866, #5758, #13040 ) ;
#2862 = CARTESIAN_POINT ( 'NONE',  ( 4.197478902586910365, -0.8524102783748742640, -3.505063281295481392 ) ) ;
#2863 = FACE_OUTER_BOUND ( 'NONE', #10572, .T. ) ;
#2864 = CARTESIAN_POINT ( 'NONE',  ( -1.040834085586084257E-13, 4.862606272033151100, -3.745885042887441063 ) ) ;
#2865 = DIRECTION ( 'NONE',  ( 1.000000000000000000, 0.000000000000000000, 0.000000000000000000 ) ) ;
#2866 = MECHANICAL_DESIGN_GEOMETRIC_PRESENTATION_REPRESENTATION (  '', ( #1366 ), #11878 ) ;
#2867 = EDGE_CURVE ( 'NONE', #15390, #20382, #9716, .T. ) ;
#2868 = CARTESIAN_POINT ( 'NONE',  ( 0.000000000000000000, -1.750000000000001554, 0.000000000000000000 ) ) ;
#2869 = CARTESIAN_POINT ( 'NONE',  ( -65.00000000000052580, 0.5000000000000490719, 3.000000000000002665 ) ) ;
#2870 = FACE_OUTER_BOUND ( 'NONE', #13873, .T. ) ;
#2871 = PLANE ( 'NONE',  #13409 ) ;
#2872 = ORIENTED_EDGE ( 'NONE', *, *, #13029, .F. ) ;
#2874 = ORIENTED_EDGE ( 'NONE', *, *, #21596, .T. ) ;
#2873 = ORIENTED_EDGE ( 'NONE', *, *, #15785, .T. ) ;
#2875 = EDGE_LOOP ( 'NONE', ( #16462, #11920, #15706, #980 ) ) ;
#2876 = AXIS2_PLACEMENT_3D ( 'NONE', #6450, #9751, #22799 ) ;
#2877 = EDGE_LOOP ( 'NONE', ( #3907, #14363, #14882, #229, #11491, #20883 ) ) ;
#2878 = EDGE_LOOP ( 'NONE', ( #691, #4951, #9968, #17787 ) ) ;
#2879 = VECTOR ( 'NONE', #15212, 1000.000000000000114 ) ;
#2880 = VERTEX_POINT ( 'NONE', #12280 ) ;
#2881 = CARTESIAN_POINT ( 'NONE',  ( 4.000000000000003553, 2.309401076758525573, -5.242734410091827613 ) ) ;
#2882 = DIRECTION ( 'NONE',  ( 0.000000000000000000, 0.000000000000000000, 1.000000000000000000 ) ) ;
#2883 = VERTEX_POINT ( 'NONE', #17832 ) ;
#2884 = ORIENTED_EDGE ( 'NONE', *, *, #16144, .T. ) ;
#2885 = CARTESIAN_POINT ( 'NONE',  ( 2.775557561562891351E-14, 10.49999999999998579, -2.133974596215532316 ) ) ;
#2886 = DIRECTION ( 'NONE',  ( 1.333893503340774882E-15, 2.778352770573747380E-17, 1.000000000000000000 ) ) ;
#2887 = EDGE_CURVE ( 'NONE', #5722, #22384, #2568, .T. ) ;
#2888 = DIRECTION ( 'NONE',  ( -1.613696256722611405E-16, 0.000000000000000000, 1.000000000000000000 ) ) ;
#2889 = CARTESIAN_POINT ( 'NONE',  ( 77.42435809754135789, -10.99999999999981526, 6.500000000000123457 ) ) ;
#2890 = DIRECTION ( 'NONE',  ( 2.013525853228508439E-32, 6.779273404243028164E-31, -1.000000000000000000 ) ) ;
#2891 = DIRECTION ( 'NONE',  ( 0.6819983600625060260, 0.7313537016191635765, 6.106365041599011361E-16 ) ) ;
#2892 = ADVANCED_FACE ( 'NONE', ( #10413 ), #19109, .T. ) ;
#2893 = CARTESIAN_POINT ( 'NONE',  ( -50.65685424949267457, 7.200000000000018829, -7.500000000000034639 ) ) ;
#2894 = CARTESIAN_POINT ( 'NONE',  ( 2.889332061078578651, 4.882140790251139784, -7.500000000000003553 ) ) ;
#2895 = DIRECTION ( 'NONE',  ( -1.000000000000000000, 1.847414967615758933E-47, -3.885780586188017323E-16 ) ) ;
#2896 = FACE_OUTER_BOUND ( 'NONE', #16298, .T. ) ;
#2897 = TOROIDAL_SURFACE ( 'NONE', #16032, 3.500000000000000000, 0.5000000000000000000 ) ;
#2898 = ORIENTED_EDGE ( 'NONE', *, *, #21021, .F. ) ;
#2899 = VECTOR ( 'NONE', #6721, 1000.000000000000000 ) ;
#2900 = EDGE_CURVE ( 'NONE', #6499, #9593, #16822, .T. ) ;
#2901 = CARTESIAN_POINT ( 'NONE',  ( 3.961551342854980451, 2.319461885623427477, 2.982574167880718274 ) ) ;
#2902 = CARTESIAN_POINT ( 'NONE',  ( -50.65685424949267457, -7.200000000000049916, 7.500000000000047962 ) ) ;
#2903 = EDGE_CURVE ( 'NONE', #17297, #5230, #1368, .T. ) ;
#2904 = EDGE_LOOP ( 'NONE', ( #17821, #20769, #8065 ) ) ;
#2905 = ADVANCED_FACE ( 'NONE', ( #8648 ), #22118, .T. ) ;
#2906 = AXIS2_PLACEMENT_3D ( 'NONE', #768, #2748, #15089 ) ;
#2907 = VERTEX_POINT ( 'NONE', #21373 ) ;
#2908 = ORIENTED_EDGE ( 'NONE', *, *, #567, .F. ) ;
#2909 = PRODUCT ( 'hex flange nut gradea_iso_ISO - 4161 - M5 - N', 'hex flange nut gradea_iso_ISO - 4161 - M5 - N', '', ( #7536 ) ) ;
#2910 = ORIENTED_EDGE ( 'NONE', *, *, #4920, .F. ) ;
#2911 = DIRECTION ( 'NONE',  ( 0.000000000000000000, 3.382522293539643228E-32, 1.000000000000000000 ) ) ;
#2912 = DIRECTION ( 'NONE',  ( 7.860214984770699307E-18, -1.409037165336591006E-16, -1.000000000000000000 ) ) ;
#2913 = VERTEX_POINT ( 'NONE', #5248 ) ;
#2914 = CIRCLE ( 'NONE', #7798, 0.5000000000000004441 ) ;
#2915 = DIRECTION ( 'NONE',  ( 0.000000000000000000, -1.000000000000000000, 0.000000000000000000 ) ) ;
#2916 = CARTESIAN_POINT ( 'NONE',  ( -53.99613665484953628, -0.5000000000001045830, -13.19342998475053719 ) ) ;
#2917 = TOROIDAL_SURFACE ( 'NONE', #23220, 5.500000000000007994, 0.5000000000000000000 ) ;
#2918 = CARTESIAN_POINT ( 'NONE',  ( 3.806834918298643178, -3.031088913245532979, 1.749999999999997113 ) ) ;
#2919 = ADVANCED_FACE ( 'NONE', ( #10641 ), #1710, .F. ) ;
#2920 = EDGE_CURVE ( 'NONE', #12385, #6815, #20246, .T. ) ;
#2921 = LINE ( 'NONE', #1166, #19297 ) ;
#2922 = DIRECTION ( 'NONE',  ( -0.7313537016191765661, -0.6819983600624919262, 1.280489736994879814E-15 ) ) ;
#2923 = AXIS2_PLACEMENT_3D ( 'NONE', #20338, #20108, #21872 ) ;
#2924 = CARTESIAN_POINT ( 'NONE',  ( -8.725359747074515226, -0.4999999928004963401, 6.816426071237475348 ) ) ;
#2925 = LINE ( 'NONE', #17141, #19348 ) ;
#2926 = AXIS2_PLACEMENT_3D ( 'NONE', #735, #6146, #9906 ) ;
#2927 = LINE ( 'NONE', #10450, #21716 ) ;
#2928 = DIRECTION ( 'NONE',  ( -0.7313537016191730133, 0.6819983600624959230, -5.924440990721418971E-17 ) ) ;
#2929 = CARTESIAN_POINT ( 'NONE',  ( 2.000000000000029310, 3.464101615137740175, 0.000000000000000000 ) ) ;
#2930 = EDGE_CURVE ( 'NONE', #3151, #13641, #2049, .T. ) ;
#2932 = CIRCLE ( 'NONE', #16791, 0.5000000000000004441 ) ;
#2931 = CARTESIAN_POINT ( 'NONE',  ( -95.20000000000064233, 3.200000000000015277, 1.000000000000014655 ) ) ;
#2933 = EDGE_CURVE ( 'NONE', #22474, #3643, #9233, .T. ) ;
#2934 = DIRECTION ( 'NONE',  ( 1.000000000000000000, 5.598259082250514647E-17, 3.330669073875432643E-16 ) ) ;
#2935 = CIRCLE ( 'NONE', #23236, 5.500000000000032863 ) ;
#2936 = ORIENTED_EDGE ( 'NONE', *, *, #2964, .T. ) ;
#2937 = EDGE_CURVE ( 'NONE', #5312, #2822, #19856, .T. ) ;
#2938 = CIRCLE ( 'NONE', #5560, 2.549999999999998490 ) ;
#2939 = CONTEXT_DEPENDENT_SHAPE_REPRESENTATION ( #1730, #11722 ) ;
#2940 = ORIENTED_EDGE ( 'NONE', *, *, #10960, .F. ) ;
#2942 = AXIS2_PLACEMENT_3D ( 'NONE', #22696, #15613, #17138 ) ;
#2941 =( REPRESENTATION_RELATIONSHIP ('NONE','NONE', #19450, #16457 ) REPRESENTATION_RELATIONSHIP_WITH_TRANSFORMATION ( #595 )SHAPE_REPRESENTATION_RELATIONSHIP( ) );
#2943 = AXIS2_PLACEMENT_3D ( 'NONE', #4719, #11775, #10135 ) ;
#2945 = ORIENTED_EDGE ( 'NONE', *, *, #22642, .F. ) ;
#2944 = ORIENTED_EDGE ( 'NONE', *, *, #12592, .F. ) ;
#2946 = CIRCLE ( 'NONE', #8960, 0.5000000000000004441 ) ;
#2947 = FACE_OUTER_BOUND ( 'NONE', #5917, .T. ) ;
#2948 = DIRECTION ( 'NONE',  ( -1.110223024625150131E-16, 1.000000000000000000, -6.902532920683853297E-31 ) ) ;
#2949 = DIRECTION ( 'NONE',  ( 2.013525853228507892E-32, 6.902532920683810383E-31, -1.000000000000000000 ) ) ;
#2950 = VERTEX_POINT ( 'NONE', #20058 ) ;
#2951 = DIRECTION ( 'NONE',  ( 0.000000000000000000, 0.000000000000000000, 1.000000000000000000 ) ) ;
#2952 = DIRECTION ( 'NONE',  ( 1.000000000000000000, 1.910522504832140594E-31, -5.551115123125818447E-17 ) ) ;
#2953 = CARTESIAN_POINT ( 'NONE',  ( -2.296348136192898792, 1.454515171358711889, 4.749999999999999112 ) ) ;
#2954 = CARTESIAN_POINT ( 'NONE',  ( 3.679171394225956515, 2.494631558665878046, -0.3503314178412145763 ) ) ;
#2955 = CARTESIAN_POINT ( 'NONE',  ( -2.000000000000015543, -3.464101615137743728, -5.600000000000000533 ) ) ;
#2956 = AXIS2_PLACEMENT_3D ( 'NONE', #18708, #14833, #22011 ) ;
#2957 = DIRECTION ( 'NONE',  ( 0.7071067811865485719, -0.7071067811865464625, -1.010793663541191362E-16 ) ) ;
#2958 = EDGE_CURVE ( 'NONE', #10026, #3117, #17998, .T. ) ;
#2959 = CARTESIAN_POINT ( 'NONE',  ( -7.000000000000020428, -8.000000000000003553, 12.24999999999999645 ) ) ;
#2960 = CIRCLE ( 'NONE', #14974, 2.250000000000003553 ) ;
#2961 = DIRECTION ( 'NONE',  ( -1.000000000000000000, 1.550910762415513985E-16, 3.012982189080959477E-32 ) ) ;
#2962 = AXIS2_PLACEMENT_3D ( 'NONE', #1115, #19095, #20524 ) ;
#2963 = DIRECTION ( 'NONE',  ( 0.000000000000000000, 0.000000000000000000, 1.000000000000000000 ) ) ;
#2964 = EDGE_CURVE ( 'NONE', #8098, #21208, #18288, .T. ) ;
#2965 = EDGE_CURVE ( 'NONE', #8517, #6969, #8583, .T. ) ;
#2966 = ORIENTED_EDGE ( 'NONE', *, *, #9531, .T. ) ;
#2967 = DIRECTION ( 'NONE',  ( -0.7296441571687829475, -0.6838270277705150724, 1.413418879721835175E-16 ) ) ;
#2969 = ORIENTED_EDGE ( 'NONE', *, *, #6054, .T. ) ;
#2968 = ORIENTED_EDGE ( 'NONE', *, *, #10105, .T. ) ;
#2970 = VERTEX_POINT ( 'NONE', #5837 ) ;
#2972 = ORIENTED_EDGE ( 'NONE', *, *, #3067, .F. ) ;
#2971 = ORIENTED_EDGE ( 'NONE', *, *, #21187, .F. ) ;
#2973 = ORIENTED_EDGE ( 'NONE', *, *, #1153, .T. ) ;
#2974 = CARTESIAN_POINT ( 'NONE',  ( 29.00000000029184832, 16.99999999900385461, -25.50000000000000355 ) ) ;
#2975 = CARTESIAN_POINT ( 'NONE',  ( 2.775557561562891351E-14, 0.2500000000000106581, -10.43301270189220276 ) ) ;
#2976 = DIRECTION ( 'NONE',  ( -1.000000000000000000, 1.550910762415516450E-16, 0.000000000000000000 ) ) ;
#2977 = TOROIDAL_SURFACE ( 'NONE', #16104, 6.500000000000000888, 0.5000000000000000000 ) ;
#2978 = AXIS2_PLACEMENT_3D ( 'NONE', #20209, #9489, #16529 ) ;
#2979 = CARTESIAN_POINT ( 'NONE',  ( -4.330127018922199866, 4.999999999999920952, 7.500000000000007105 ) ) ;
#2980 = CARTESIAN_POINT ( 'NONE',  ( -55.25320565519145788, -2.700000000000049472, 8.000000000000062172 ) ) ;
#2981 = CARTESIAN_POINT ( 'NONE',  ( -8.037202331403086930, -2.196591282338350659, 7.528743044528591888 ) ) ;
#2982 = DIRECTION ( 'NONE',  ( 0.7071067811865491270, 0.7071067811865461294, 1.565905175853767167E-16 ) ) ;
#2983 = DIRECTION ( 'NONE',  ( -9.121204216617949000E-31, -1.000000000000000000, 6.982962677686261977E-15 ) ) ;
#2984 = CARTESIAN_POINT ( 'NONE',  ( 3.999999999999989786, -2.309401076758549998, -5.242734410091827613 ) ) ;
#2985 = CARTESIAN_POINT ( 'NONE',  ( -2.344047193898689763, -3.265465875126513318, -7.162087085508733993E-14 ) ) ;
#2986 = DIRECTION ( 'NONE',  ( 0.000000000000000000, 0.000000000000000000, 1.000000000000000000 ) ) ;
#2987 = EDGE_CURVE ( 'NONE', #7794, #19662, #2735, .T. ) ;
#2988 =( GEOMETRIC_REPRESENTATION_CONTEXT ( 3 ) GLOBAL_UNCERTAINTY_ASSIGNED_CONTEXT ( ( #2519 ) ) GLOBAL_UNIT_ASSIGNED_CONTEXT ( ( #17091, #13586, #9942 ) ) REPRESENTATION_CONTEXT ( 'NONE', 'WORKASPACE' ) );
#2989 = CARTESIAN_POINT ( 'NONE',  ( -42.54314575050793934, 7.999999999999992895, -7.500000000000062172 ) ) ;
#2990 = LINE ( 'NONE', #10160, #21709 ) ;
#2991 = CARTESIAN_POINT ( 'NONE',  ( -6.839530184912446131, 13.99859551563898563, -26.98838964695894660 ) ) ;
#2992 = LINE ( 'NONE', #22172, #11157 ) ;
#2993 = EDGE_CURVE ( 'NONE', #16467, #16377, #3582, .T. ) ;
#2994 = ORIENTED_EDGE ( 'NONE', *, *, #15001, .T. ) ;
#2995 = PRODUCT_DEFINITION_CONTEXT ( 'detailed design', #2765, 'design' ) ;
#2996 =( NAMED_UNIT ( * ) PLANE_ANGLE_UNIT ( ) SI_UNIT ( $, .RADIAN. ) );
#2998 = ORIENTED_EDGE ( 'NONE', *, *, #16403, .F. ) ;
#2997 = EDGE_LOOP ( 'NONE', ( #23121, #6037, #23053, #17300 ) ) ;
#2999 = ORIENTED_EDGE ( 'NONE', *, *, #16197, .T. ) ;
#3000 = VERTEX_POINT ( 'NONE', #16276 ) ;
#3001 = ORIENTED_EDGE ( 'NONE', *, *, #16818, .F. ) ;
#3002 = AXIS2_PLACEMENT_3D ( 'NONE', #857, #8025, #2847 ) ;
#3003 = ADVANCED_FACE ( 'NONE', ( #12759 ), #16461, .T. ) ;
#3004 = VERTEX_POINT ( 'NONE', #13218 ) ;
#3005 = LINE ( 'NONE', #11584, #12546 ) ;
#3006 = DIRECTION ( 'NONE',  ( 0.8660254037844371533, 0.5000000000000025535, 0.000000000000000000 ) ) ;
#3007 = ORIENTED_EDGE ( 'NONE', *, *, #11484, .F. ) ;
#3008 = FACE_OUTER_BOUND ( 'NONE', #1129, .T. ) ;
#3009 = CARTESIAN_POINT ( 'NONE',  ( 1.393927851585456290, -4.043713361053605126, -3.526374918436861350 ) ) ;
#3010 = DIRECTION ( 'NONE',  ( 1.000000000000000000, 0.000000000000000000, 0.000000000000000000 ) ) ;
#3011 = LINE ( 'NONE', #12518, #21744 ) ;
#3012 = CARTESIAN_POINT ( 'NONE',  ( 54.42435809754113052, -4.000000000000003553, -6.000000000000012434 ) ) ;
#3013 = DIRECTION ( 'NONE',  ( -1.733449886265891589E-32, 4.190823558986610327E-31, -1.000000000000000000 ) ) ;
#3014 = CARTESIAN_POINT ( 'NONE',  ( -4.000000000000095035, 1.563622288139215888, -0.2253451193528957786 ) ) ;
#3015 = DIRECTION ( 'NONE',  ( -7.860214984770699307E-18, 1.409037165336591006E-16, 1.000000000000000000 ) ) ;
#3016 = TOROIDAL_SURFACE ( 'NONE', #9030, 9.499999999999998224, 0.5000000000000000000 ) ;
#3017 = DIRECTION ( 'NONE',  ( -1.000000000000000000, -1.479114197289397135E-31, -5.916456789157588541E-31 ) ) ;
#3018 = DIRECTION ( 'NONE',  ( -0.7071067811865474617, 0.7071067811865474617, -0.000000000000000000 ) ) ;
#3019 = ORIENTED_EDGE ( 'NONE', *, *, #19333, .F. ) ;
#3020 = FILL_AREA_STYLE ('',( #11600 ) ) ;
#3021 = LINE ( 'NONE', #4544, #13855 ) ;
#3022 = CARTESIAN_POINT ( 'NONE',  ( 12.84999999999997300, -13.50000000000003020, 5.750000000000047073 ) ) ;
#3023 = ORIENTED_EDGE ( 'NONE', *, *, #23047, .F. ) ;
#3024 = ADVANCED_FACE ( 'NONE', ( #189 ), #16504, .T. ) ;
#3025 = ADVANCED_BREP_SHAPE_REPRESENTATION ( '', ( #5146, #22115 ), #18753 ) ;
#3026 = ORIENTED_EDGE ( 'NONE', *, *, #15093, .T. ) ;
#3027 = ORIENTED_EDGE ( 'NONE', *, *, #4619, .F. ) ;
#3028 = ORIENTED_EDGE ( 'NONE', *, *, #22353, .F. ) ;
#3029 = ORIENTED_EDGE ( 'NONE', *, *, #474, .F. ) ;
#3030 = ADVANCED_FACE ( 'NONE', ( #2283 ), #5219, .T. ) ;
#3031 = CARTESIAN_POINT ( 'NONE',  ( 4.151274195509674136, 2.039912954708746007, 3.533232880573493162 ) ) ;
#3032 = FACE_OUTER_BOUND ( 'NONE', #7451, .T. ) ;
#3033 = ORIENTED_EDGE ( 'NONE', *, *, #13323, .F. ) ;
#3034 = AXIS2_PLACEMENT_3D ( 'NONE', #2629, #9804, #20638 ) ;
#3035 = FACE_OUTER_BOUND ( 'NONE', #12793, .T. ) ;
#3036 = CARTESIAN_POINT ( 'NONE',  ( 2.500000000000002220, 0.000000000000000000, -5.600000000000000533 ) ) ;
#3037 = CARTESIAN_POINT ( 'NONE',  ( 4.071447262713884463, -2.020725942163688504, 3.499999999999997780 ) ) ;
#3038 = ADVANCED_FACE ( 'NONE', ( #648 ), #21387, .T. ) ;
#3039 = DIRECTION ( 'NONE',  ( -1.000000000000000000, 0.000000000000000000, 0.000000000000000000 ) ) ;
#3040 = DIRECTION ( 'NONE',  ( -4.844685039213900252E-16, -1.201780285297635172E-31, 1.000000000000000000 ) ) ;
#3041 = B_SPLINE_CURVE_WITH_KNOTS ( 'NONE', 3,
 ( #19714, #22894, #8886, #10528 ),
 .UNSPECIFIED., .F., .F.,
 ( 4, 4 ),
 ( 0.0007727519425873948704, 0.0007833511101368439283 ),
 .UNSPECIFIED. ) ;
#3042 = DIRECTION ( 'NONE',  ( 0.000000000000000000, 0.000000000000000000, -1.000000000000000000 ) ) ;
#3043 = EDGE_CURVE ( 'NONE', #20178, #6413, #22167, .T. ) ;
#3044 = CARTESIAN_POINT ( 'NONE',  ( 124.5000000000017195, -4.500000000000059508, 1.387778780781445676E-14 ) ) ;
#3045 = CARTESIAN_POINT ( 'NONE',  ( -1.418636431716181459E-15, -3.375361811986499205, 1.153701847711630091 ) ) ;
#3046 = DIRECTION ( 'NONE',  ( 1.000000000000000000, 5.598259082250514647E-17, 3.330669073875432643E-16 ) ) ;
#3047 = CARTESIAN_POINT ( 'NONE',  ( 1.387778780781445676E-14, 4.618802153517020059, -0.3572655899081733644 ) ) ;
#3048 = DIRECTION ( 'NONE',  ( -1.066786462891689527E-26, -6.656013887802287108E-31, -1.000000000000000000 ) ) ;
#3049 = PLANE ( 'NONE',  #5194 ) ;
#3050 = AXIS2_PLACEMENT_3D ( 'NONE', #14118, #1192, #3307 ) ;
#3051 = ORIENTED_EDGE ( 'NONE', *, *, #17748, .F. ) ;
#3052 = ADVANCED_FACE ( 'NONE', ( #10872 ), #18065, .T. ) ;
#3053 = EDGE_CURVE ( 'NONE', #18271, #22610, #763, .T. ) ;
#3054 = ORIENTED_EDGE ( 'NONE', *, *, #52, .T. ) ;
#3055 = ADVANCED_FACE ( 'NONE', ( #2863 ), #11908, .T. ) ;
#3057 = ORIENTED_EDGE ( 'NONE', *, *, #22635, .T. ) ;
#3056 = ORIENTED_EDGE ( 'NONE', *, *, #15395, .T. ) ;
#3058 = DIRECTION ( 'NONE',  ( 2.013525853228507892E-32, 6.902532920683810383E-31, -1.000000000000000000 ) ) ;
#3059 = DIRECTION ( 'NONE',  ( 1.000000000000000000, -4.190823558986610327E-31, 1.733449886265890494E-32 ) ) ;
#3060 = CARTESIAN_POINT ( 'NONE',  ( -6.147973203409641485, 36.05667699661070458, -26.27430804596576408 ) ) ;
#3062 = VERTEX_POINT ( 'NONE', #8401 ) ;
#3061 = EDGE_CURVE ( 'NONE', #20416, #16256, #4078, .T. ) ;
#3063 = DIRECTION ( 'NONE',  ( 1.000000000000000000, 0.000000000000000000, 0.000000000000000000 ) ) ;
#3064 = AXIS2_PLACEMENT_3D ( 'NONE', #5503, #16413, #12662 ) ;
#3065 = AXIS2_PLACEMENT_3D ( 'NONE', #20550, #11940, #16991 ) ;
#3066 = CARTESIAN_POINT ( 'NONE',  ( 24.75000000000000355, 2.000000000000029310, -2.000000000000005329 ) ) ;
#3067 = EDGE_CURVE ( 'NONE', #16088, #15251, #9680, .T. ) ;
#3068 = CARTESIAN_POINT ( 'NONE',  ( -4.499999999708154341, 35.49999999900384751, -25.50000000000000000 ) ) ;
#3069 = DIRECTION ( 'NONE',  ( -9.121204216617949000E-31, -1.000000000000000000, 6.982962677686261977E-15 ) ) ;
#3070 = CARTESIAN_POINT ( 'NONE',  ( 6.248040462138590701E-13, -4.796980096169678021, -3.721999068284442380 ) ) ;
#3071 = DIRECTION ( 'NONE',  ( 1.550910762415566494E-16, 1.000000000000000000, -8.135128085091684243E-31 ) ) ;
#3072 = CYLINDRICAL_SURFACE ( 'NONE', #2182, 0.5000000000000017764 ) ;
#3073 = CARTESIAN_POINT ( 'NONE',  ( -4.663920683512478682, 0.7500000000000504041, -2.263176076085167132 ) ) ;
#3074 = CARTESIAN_POINT ( 'NONE',  ( 3.000000000291852764, 42.99999999900385461, -26.00000000000000000 ) ) ;
#3075 = CARTESIAN_POINT ( 'NONE',  ( 4.071447262713884463, -4.041451884327383226, 0.000000000000000000 ) ) ;
#3076 = ADVANCED_FACE ( 'NONE', ( #8160 ), #13459, .T. ) ;
#3077 = EDGE_CURVE ( 'NONE', #15429, #20382, #22076, .T. ) ;
#3078 = ORIENTED_EDGE ( 'NONE', *, *, #12818, .T. ) ;
#3079 = EDGE_CURVE ( 'NONE', #7097, #4023, #18164, .T. ) ;
#3080 = DIRECTION ( 'NONE',  ( 1.357283353553633170E-16, 1.055997096961978158E-16, 1.000000000000000000 ) ) ;
#3081 = CIRCLE ( 'NONE', #6087, 5.749999999999992006 ) ;
#3082 = AXIS2_PLACEMENT_3D ( 'NONE', #2448, #16902, #4440 ) ;
#3084 = ORIENTED_EDGE ( 'NONE', *, *, #6771, .F. ) ;
#3083 = VERTEX_POINT ( 'NONE', #17082 ) ;
#3085 = VERTEX_POINT ( 'NONE', #15328 ) ;
#3087 = ORIENTED_EDGE ( 'NONE', *, *, #10236, .F. ) ;
#3086 = ORIENTED_EDGE ( 'NONE', *, *, #18849, .T. ) ;
#3088 = ORIENTED_EDGE ( 'NONE', *, *, #9695, .F. ) ;
#3089 = ADVANCED_FACE ( 'NONE', ( #2511 ), #15795, .T. ) ;
#3090 = CARTESIAN_POINT ( 'NONE',  ( 0.000000000000000000, -1.750000000000001554, 0.000000000000000000 ) ) ;
#3091 = ADVANCED_FACE ( 'NONE', ( #10704 ), #12702, .T. ) ;
#3092 = FACE_BOUND ( 'NONE', #12650, .T. ) ;
#3093 = CARTESIAN_POINT ( 'NONE',  ( 12.84999999999997300, 0.000000000000000000, 1.387778780781445676E-14 ) ) ;
#3094 = ADVANCED_FACE ( 'NONE', ( #7188 ), #19649, .T. ) ;
#3095 = MECHANICAL_DESIGN_GEOMETRIC_PRESENTATION_REPRESENTATION (  '', ( #19997 ), #4958 ) ;
#3096 = CARTESIAN_POINT ( 'NONE',  ( 0.000000000000000000, 0.000000000000000000, -25.03750572909317285 ) ) ;
#3097 = CARTESIAN_POINT ( 'NONE',  ( -8.697224362268011433, 6.938893903907228378E-15, 6.249999999999992006 ) ) ;
#3098 = CARTESIAN_POINT ( 'NONE',  ( -8.422565759993835499, -1.999999999999987121, 6.396710472007108628 ) ) ;
#3099 = DIRECTION ( 'NONE',  ( -9.121204216617949000E-31, -1.000000000000000000, 6.982962677686276966E-15 ) ) ;
#3100 = CIRCLE ( 'NONE', #13970, 7.000000000000075495 ) ;
#3101 = CARTESIAN_POINT ( 'NONE',  ( 3.948095570616719563, 0.6965071952228556462, 3.499999999999969358 ) ) ;
#3102 = CIRCLE ( 'NONE', #14011, 2.250000000000003553 ) ;
#3103 = CARTESIAN_POINT ( 'NONE',  ( 80.49335071782266482, -7.708908342713566064, -6.500000000000047073 ) ) ;
#3104 = AXIS2_PLACEMENT_3D ( 'NONE', #2423, #433, #10891 ) ;
#3105 = FACE_OUTER_BOUND ( 'NONE', #9826, .T. ) ;
#3106 = CYLINDRICAL_SURFACE ( 'NONE', #12675, 0.5000000000000038858 ) ;
#3107 = CARTESIAN_POINT ( 'NONE',  ( 54.42435809754108078, -4.000000000000003553, 6.500000000000081712 ) ) ;
#3108 = FACE_OUTER_BOUND ( 'NONE', #1126, .T. ) ;
#3109 = PRODUCT_DEFINITION_SHAPE ( 'NONE', 'NONE',  #8624 ) ;
#3110 = EDGE_LOOP ( 'NONE', ( #13809, #15979, #12595, #2764 ) ) ;
#3111 = MECHANICAL_DESIGN_GEOMETRIC_PRESENTATION_REPRESENTATION (  '', ( #6872 ), #12107 ) ;
#3112 =( NAMED_UNIT ( * ) PLANE_ANGLE_UNIT ( ) SI_UNIT ( $, .RADIAN. ) );
#3114 = EDGE_LOOP ( 'NONE', ( #5783, #20157, #17268, #1245 ) ) ;
#3113 = ORIENTED_EDGE ( 'NONE', *, *, #20891, .T. ) ;
#3115 = ORIENTED_EDGE ( 'NONE', *, *, #20628, .T. ) ;
#3116 = EDGE_CURVE ( 'NONE', #21123, #2526, #11919, .T. ) ;
#3117 = VERTEX_POINT ( 'NONE', #5427 ) ;
#3118 = CIRCLE ( 'NONE', #849, 4.750000000000000000 ) ;
#3119 = ORIENTED_EDGE ( 'NONE', *, *, #13675, .F. ) ;
#3120 = CIRCLE ( 'NONE', #2368, 0.5000000000000004441 ) ;
#3121 = CIRCLE ( 'NONE', #8370, 0.5000000000000028866 ) ;
#3122 = TOROIDAL_SURFACE ( 'NONE', #121, 5.500000000000000000, 0.5000000000000000000 ) ;
#3123 = ORIENTED_EDGE ( 'NONE', *, *, #14408, .F. ) ;
#3124 = CARTESIAN_POINT ( 'NONE',  ( 5.600000000000000533, 4.041451884327335264, -1.734723475976807094E-14 ) ) ;
#3125 = CARTESIAN_POINT ( 'NONE',  ( -3.200000000000091660, -2.000000000000050182, -7.500000000000034639 ) ) ;
#3126 = ORIENTED_EDGE ( 'NONE', *, *, #13856, .T. ) ;
#3127 = CARTESIAN_POINT ( 'NONE',  ( -7.644579933246792969, -13.15747815713137570, 8.321099285265857404 ) ) ;
#3128 = EDGE_CURVE ( 'NONE', #15881, #7096, #4700, .T. ) ;
#3129 = CARTESIAN_POINT ( 'NONE',  ( 0.6937372685066356404, -4.453844082567806062, -3.610536846335917982 ) ) ;
#3130 = CARTESIAN_POINT ( 'NONE',  ( 4.000000000000003553, -1.933795701539624323, -5.351162342337697275 ) ) ;
#3131 = DIRECTION ( 'NONE',  ( -1.000000000000000000, -4.440892098500626162E-16, 5.551115123125782702E-16 ) ) ;
#3132 = LINE ( 'NONE', #10415, #12828 ) ;
#3133 = CARTESIAN_POINT ( 'NONE',  ( 0.000000000000000000, 0.000000000000000000, -4.000000000000000000 ) ) ;
#3134 = EDGE_CURVE ( 'NONE', #6825, #1880, #5299, .T. ) ;
#3135 =( LENGTH_UNIT ( ) NAMED_UNIT ( * ) SI_UNIT ( .MILLI., .METRE. ) );
#3136 = DIRECTION ( 'NONE',  ( 1.000000000000000000, 2.220446049250314067E-16, -5.825996348268307008E-33 ) ) ;
#3137 = CIRCLE ( 'NONE', #885, 2.500000000000015987 ) ;
#3138 = VECTOR ( 'NONE', #18, 1000.000000000000000 ) ;
#3139 = DIRECTION ( 'NONE',  ( -1.000000000000000000, 1.276756478318923119E-15, -1.387778780781436998E-15 ) ) ;
#3140 = DIRECTION ( 'NONE',  ( 0.000000000000000000, 0.000000000000000000, -1.000000000000000000 ) ) ;
#3141 = CIRCLE ( 'NONE', #1995, 0.5155456020628804703 ) ;
#3142 = VERTEX_POINT ( 'NONE', #16099 ) ;
#3143 = CIRCLE ( 'NONE', #16633, 0.4999999999999990563 ) ;
#3144 = AXIS2_PLACEMENT_3D ( 'NONE', #22974, #10258, #17429 ) ;
#3145 = SURFACE_STYLE_FILL_AREA ( #1379 ) ;
#3146 = CARTESIAN_POINT ( 'NONE',  ( 3.880206590543184841, 2.665671387532550174, 2.382921720511005592 ) ) ;
#3147 = DIRECTION ( 'NONE',  ( -1.000000000000000000, 4.190823558986610327E-31, -1.733449886265890494E-32 ) ) ;
#3148 = B_SPLINE_CURVE_WITH_KNOTS ( 'NONE', 3,
 ( #17916, #8977, #16477, #18034, #14610, #18256, #384, #12730 ),
 .UNSPECIFIED., .F., .F.,
 ( 4, 2, 2, 4 ),
 ( 0.002775112046897006395, 0.003466237704215411296, 0.004157363361533816630, 0.005539614676170626431 ),
 .UNSPECIFIED. ) ;
#3150 = ORIENTED_EDGE ( 'NONE', *, *, #1742, .T. ) ;
#3149 = VERTEX_POINT ( 'NONE', #19532 ) ;
#3151 = VERTEX_POINT ( 'NONE', #9292 ) ;
#3152 = B_SPLINE_CURVE_WITH_KNOTS ( 'NONE', 3,
 ( #4228, #11187, #20362, #2476, #5678, #22245, #2361, #15053, #9550, #16473, #20492, #9655, #7892, #6133, #9199, #13312 ),
 .UNSPECIFIED., .F., .F.,
 ( 4, 3, 3, 3, 3, 4 ),
 ( 0.000000000000000000, 3.315506744709602110E-05, 6.608280158699783688E-05, 0.0001026520855291450108, 0.0001376952025664789059, 0.0001398064759190598540 ),
 .UNSPECIFIED. ) ;
#3153 = ORIENTED_EDGE ( 'NONE', *, *, #15877, .F. ) ;
#3154 = CARTESIAN_POINT ( 'NONE',  ( 4.114405500665259119, 2.025575754679715068, 3.508400121684933204 ) ) ;
#3155 = CARTESIAN_POINT ( 'NONE',  ( 0.000000000000000000, -0.5999999999999789946, -3.054668707061614086 ) ) ;
#3156 = TOROIDAL_SURFACE ( 'NONE', #9161, 3.299999999999999822, 0.5000000000000000000 ) ;
#3157 = AXIS2_PLACEMENT_3D ( 'NONE', #17026, #940, #10642 ) ;
#3158 = CARTESIAN_POINT ( 'NONE',  ( -3.646393709166105168, -1.750000000000010214, 3.184260831324758456 ) ) ;
#3159 = AXIS2_PLACEMENT_3D ( 'NONE', #1724, #14314, #8791 ) ;
#3160 = CARTESIAN_POINT ( 'NONE',  ( 7.000000000000006217, -1.999999999999994893, 10.74999999999998224 ) ) ;
#3161 = DIRECTION ( 'NONE',  ( 3.885780586188016830E-16, 4.437342591868156373E-31, -1.000000000000000000 ) ) ;
#3162 = AXIS2_PLACEMENT_3D ( 'NONE', #576, #7741, #18336 ) ;
#3163 = CARTESIAN_POINT ( 'NONE',  ( -7.499999999999992895, -14.00000000000004441, 6.250000000000047073 ) ) ;
#3164 = CARTESIAN_POINT ( 'NONE',  ( 2.869123094150544522E-16, -14.99999999999997513, -4.750000000000013323 ) ) ;
#3165 = DIRECTION ( 'NONE',  ( -2.013525853228507892E-32, -6.902532920683810383E-31, 1.000000000000000000 ) ) ;
#3166 = CARTESIAN_POINT ( 'NONE',  ( -5.036205380386573616, -1.584759246591067594, -0.7770364038185282318 ) ) ;
#3167 = DIRECTION ( 'NONE',  ( 1.000000000000000000, -4.437342591868175641E-31, 3.330669073875457788E-16 ) ) ;
#3168 = CARTESIAN_POINT ( 'NONE',  ( -42.54314575050785407, -5.300000000000020250, 8.000000000000007105 ) ) ;
#3169 = DIRECTION ( 'NONE',  ( -1.000000000000000000, 0.000000000000000000, 0.000000000000000000 ) ) ;
#3170 = CARTESIAN_POINT ( 'NONE',  ( 4.749999999999986677, -2.109423746787803343E-15, -3.733602117766269525E-17 ) ) ;
#3171 = EDGE_CURVE ( 'NONE', #17679, #9575, #19992, .T. ) ;
#3172 = AXIS2_PLACEMENT_3D ( 'NONE', #7552, #18480, #11190 ) ;
#3173 = DIRECTION ( 'NONE',  ( -1.581383788144386089E-16, 0.000000000000000000, 1.000000000000000000 ) ) ;
#3174 = VECTOR ( 'NONE', #17205, 1000.000000000000000 ) ;
#3175 = ORIENTED_EDGE ( 'NONE', *, *, #12553, .F. ) ;
#3176 = AXIS2_PLACEMENT_3D ( 'NONE', #18080, #11005, #9371 ) ;
#3177 = CONTEXT_DEPENDENT_SHAPE_REPRESENTATION ( #6556, #9853 ) ;
#3178 = ORIENTED_EDGE ( 'NONE', *, *, #4244, .F. ) ;
#3179 = LINE ( 'NONE', #14226, #13647 ) ;
#3181 = ORIENTED_EDGE ( 'NONE', *, *, #15093, .F. ) ;
#3180 = VERTEX_POINT ( 'NONE', #9178 ) ;
#3182 = ADVANCED_FACE ( 'NONE', ( #3753 ), #19067, .T. ) ;
#3183 = CARTESIAN_POINT ( 'NONE',  ( -47.47487373415315659, -4.018019484660608320, -8.000000000000007105 ) ) ;
#3184 = ORIENTED_EDGE ( 'NONE', *, *, #6586, .F. ) ;
#3185 = CARTESIAN_POINT ( 'NONE',  ( 2.498001805406602216E-13, 0.000000000000000000, 6.500000000000103029 ) ) ;
#3186 = CARTESIAN_POINT ( 'NONE',  ( -64.00000000000045475, 3.200000000000057021, -1.999999999999974021 ) ) ;
#3187 = CIRCLE ( 'NONE', #3172, 2.550000000000012701 ) ;
#3188 = ORIENTED_EDGE ( 'NONE', *, *, #5833, .T. ) ;
#3189 = FACE_OUTER_BOUND ( 'NONE', #8380, .T. ) ;
#3190 = CARTESIAN_POINT ( 'NONE',  ( 2.742413778650726108, -1.325747111984059590, 4.749999999999997335 ) ) ;
#3191 = B_SPLINE_CURVE_WITH_KNOTS ( 'NONE', 3,
 ( #22659, #11590, #15114, #13246, #11934, #19013, #22310, #4410, #18777, #2654, #9958, #4764, #22421, #6197, #2776, #20430 ),
 .UNSPECIFIED., .F., .F.,
 ( 4, 3, 3, 3, 3, 4 ),
 ( 0.000000000000000000, 3.315506744709155554E-05, 6.608280158698813327E-05, 0.0001026520855291346973, 0.0001376952025664800172, 0.0001398064759190610737 ),
 .UNSPECIFIED. ) ;
#3192 = CARTESIAN_POINT ( 'NONE',  ( 6.500000000000227374, 2.500000000000168754, 4.163336342344337027E-14 ) ) ;
#3193 = MECHANICAL_DESIGN_GEOMETRIC_PRESENTATION_REPRESENTATION (  '', ( #191 ), #16682 ) ;
#3194 = CARTESIAN_POINT ( 'NONE',  ( 4.071447262713884463, -2.020725942163709377, 3.500000000000003109 ) ) ;
#3195 = EDGE_CURVE ( 'NONE', #9560, #8464, #13662, .T. ) ;
#3196 = DIRECTION ( 'NONE',  ( 3.885780586188016830E-16, 4.437342591868156373E-31, -1.000000000000000000 ) ) ;
#3197 = DIRECTION ( 'NONE',  ( 2.710505431213761578E-16, -1.000000000000000000, 7.518830502887770522E-31 ) ) ;
#3198 = CARTESIAN_POINT ( 'NONE',  ( -3.200000000000133404, 1.999999999999953149, -8.000000000000035527 ) ) ;
#3199 = CARTESIAN_POINT ( 'NONE',  ( -47.82842712474649716, 4.371572875253824542, 8.000000000000021316 ) ) ;
#3200 = ADVANCED_FACE ( 'NONE', ( #7078 ), #14474, .F. ) ;
#3201 = DIRECTION ( 'NONE',  ( -4.336808689941983223E-16, 0.000000000000000000, 1.000000000000000000 ) ) ;
#3202 = CARTESIAN_POINT ( 'NONE',  ( 4.142654963991858175, -4.070796997468697498, -4.252513780320472990E-18 ) ) ;
#3203 = EDGE_LOOP ( 'NONE', ( #22259, #4579, #1179 ) ) ;
#3204 = AXIS2_PLACEMENT_3D ( 'NONE', #6832, #3539, #8946 ) ;
#3205 = ADVANCED_FACE ( 'NONE', ( #17888 ), #18235, .T. ) ;
#3206 = PRODUCT_CONTEXT ( 'NONE', #11146, 'mechanical' ) ;
#3207 = ADVANCED_FACE ( 'NONE', ( #7307 ), #14583, .F. ) ;
#3209 = ORIENTED_EDGE ( 'NONE', *, *, #3680, .F. ) ;
#3208 = ORIENTED_EDGE ( 'NONE', *, *, #13713, .T. ) ;
#3210 = ORIENTED_EDGE ( 'NONE', *, *, #1173, .F. ) ;
#3212 = VERTEX_POINT ( 'NONE', #5882 ) ;
#3211 = ORIENTED_EDGE ( 'NONE', *, *, #15485, .T. ) ;
#3213 = DIRECTION ( 'NONE',  ( 1.331202777560457422E-30, 1.000000000000000000, -7.395570986446985676E-31 ) ) ;
#3214 = CARTESIAN_POINT ( 'NONE',  ( 2.775557561562891351E-14, 8.500000000000003553, -12.50000000000001066 ) ) ;
#3215 = DIRECTION ( 'NONE',  ( 0.000000000000000000, 0.000000000000000000, 1.000000000000000000 ) ) ;
#3216 = CARTESIAN_POINT ( 'NONE',  ( 37.00000000000014211, 0.000000000000000000, -9.999999999999980460 ) ) ;
#3217 = LINE ( 'NONE', #1218, #1026 ) ;
#3218 = DIRECTION ( 'NONE',  ( -1.000000000000000000, 4.440892098500637995E-16, 0.000000000000000000 ) ) ;
#3219 = EDGE_CURVE ( 'NONE', #13762, #18075, #2148, .T. ) ;
#3220 = CARTESIAN_POINT ( 'NONE',  ( 36.00000000029184832, 5.999999999003851059, -28.99999999999999645 ) ) ;
#3221 = EDGE_CURVE ( 'NONE', #10966, #5384, #3668, .T. ) ;
#3222 = EDGE_CURVE ( 'NONE', #21815, #20382, #588, .T. ) ;
#3223 = CARTESIAN_POINT ( 'NONE',  ( 88.75737332930596324, -13.02760560296348302, -6.499999999999964473 ) ) ;
#3224 = FACE_BOUND ( 'NONE', #18759, .T. ) ;
#3225 = AXIS2_PLACEMENT_3D ( 'NONE', #3185, #10342, #5643 ) ;
#3226 = FACE_OUTER_BOUND ( 'NONE', #22419, .T. ) ;
#3227 = FACE_BOUND ( 'NONE', #18498, .T. ) ;
#3228 = DIRECTION ( 'NONE',  ( -1.000000000000000000, -1.479114197289388027E-30, 2.013525853228518840E-32 ) ) ;
#3229 = CARTESIAN_POINT ( 'NONE',  ( -42.54314575050793934, 7.499999999999992895, 8.000000000000035527 ) ) ;
#3230 = CARTESIAN_POINT ( 'NONE',  ( 29.00000000029184832, 16.99999999900385461, -19.00000000000000355 ) ) ;
#3231 = EDGE_CURVE ( 'NONE', #22993, #18159, #12287, .T. ) ;
#3232 = CARTESIAN_POINT ( 'NONE',  ( 108.2426266706970637, -13.02760560296348302, 6.500000000000019540 ) ) ;
#3233 = EDGE_LOOP ( 'NONE', ( #16430, #6729, #15172, #743 ) ) ;
#3234 = ADVANCED_FACE ( 'NONE', ( #18580 ), #13052, .F. ) ;
#3235 = SURFACE_STYLE_USAGE ( .BOTH. , #14389 ) ;
#3236 = B_SPLINE_CURVE_WITH_KNOTS ( 'NONE', 3,
 ( #16776, #9398, #9278, #18224, #21984, #5641, #18102, #1974 ),
 .UNSPECIFIED., .F., .F.,
 ( 4, 2, 2, 4 ),
 ( 0.000000000000000000, 0.0006328062630452634943, 0.001265612526090526989, 0.002531225052181053543 ),
 .UNSPECIFIED. ) ;
#3238 = ORIENTED_EDGE ( 'NONE', *, *, #16415, .T. ) ;
#3237 = VERTEX_POINT ( 'NONE', #9412 ) ;
#3239 = ORIENTED_EDGE ( 'NONE', *, *, #8923, .F. ) ;
#3240 = ORIENTED_EDGE ( 'NONE', *, *, #9671, .T. ) ;
#3241 = ORIENTED_EDGE ( 'NONE', *, *, #21339, .T. ) ;
#3242 = ORIENTED_EDGE ( 'NONE', *, *, #14791, .T. ) ;
#3243 = CARTESIAN_POINT ( 'NONE',  ( 3.000000000291852764, 42.99999999900385461, -19.49999999999998934 ) ) ;
#3244 = AXIS2_PLACEMENT_3D ( 'NONE', #20977, #10035, #8389 ) ;
#3245 = PLANE ( 'NONE',  #6123 ) ;
#3246 = ORIENTED_EDGE ( 'NONE', *, *, #11348, .T. ) ;
#3247 = CARTESIAN_POINT ( 'NONE',  ( -7.909386411297020025, -13.36290293203342650, 7.731447622712522616 ) ) ;
#3248 = LINE ( 'NONE', #1250, #17370 ) ;
#3249 = AXIS2_PLACEMENT_3D ( 'NONE', #15160, #15387, #22575 ) ;
#3250 = CARTESIAN_POINT ( 'NONE',  ( -1.391697335622858356, -4.043246145443450068, -3.503898532754396555 ) ) ;
#3251 = CARTESIAN_POINT ( 'NONE',  ( 5.599999999999994316, 4.041451884327383226, 0.000000000000000000 ) ) ;
#3252 = CARTESIAN_POINT ( 'NONE',  ( 42.50000000000012079, 10.49999999999999822, -0.4999999999999865663 ) ) ;
#3253 = DIRECTION ( 'NONE',  ( -0.000000000000000000, 0.000000000000000000, 1.000000000000000000 ) ) ;
#3254 = CYLINDRICAL_SURFACE ( 'NONE', #9503, 0.5000000000000004441 ) ;
#3255 = PRESENTATION_STYLE_ASSIGNMENT (( #1712 ) ) ;
#3256 = CARTESIAN_POINT ( 'NONE',  ( 0.000000000000000000, 0.000000000000000000, 3.469446951953614189E-15 ) ) ;
#3257 = CARTESIAN_POINT ( 'NONE',  ( 0.000000000000000000, 0.000000000000000000, 0.000000000000000000 ) ) ;
#3258 = EDGE_CURVE ( 'NONE', #12387, #22557, #8172, .T. ) ;
#3259 = DIRECTION ( 'NONE',  ( -0.000000000000000000, -0.000000000000000000, 1.000000000000000000 ) ) ;
#3260 = ORIENTED_EDGE ( 'NONE', *, *, #6238, .T. ) ;
#3261 = CIRCLE ( 'NONE', #5128, 0.5000000000000029976 ) ;
#3262 = CARTESIAN_POINT ( 'NONE',  ( 4.050823680195218657, 3.779313952391380571, -0.5899027668435183891 ) ) ;
#3263 = FACE_OUTER_BOUND ( 'NONE', #12746, .T. ) ;
#3265 = ORIENTED_EDGE ( 'NONE', *, *, #6149, .F. ) ;
#3264 = ORIENTED_EDGE ( 'NONE', *, *, #13555, .F. ) ;
#3266 = EDGE_CURVE ( 'NONE', #4468, #5612, #16793, .T. ) ;
#3267 = AXIS2_PLACEMENT_3D ( 'NONE', #4885, #10303, #21135 ) ;
#3268 = ORIENTED_EDGE ( 'NONE', *, *, #21927, .T. ) ;
#3269 = ORIENTED_EDGE ( 'NONE', *, *, #1818, .F. ) ;
#3270 = VERTEX_POINT ( 'NONE', #18348 ) ;
#3271 = DIRECTION ( 'NONE',  ( 3.885780586188016830E-16, 4.437342591868156373E-31, -1.000000000000000000 ) ) ;
#3272 = CARTESIAN_POINT ( 'NONE',  ( 77.42435809754134368, -10.99999999999981526, -6.000000000000047073 ) ) ;
#3273 = LINE ( 'NONE', #14084, #6860 ) ;
#3274 = DIRECTION ( 'NONE',  ( 1.134196829589822059E-15, 6.741645191078037727E-32, -1.000000000000000000 ) ) ;
#3275 = CARTESIAN_POINT ( 'NONE',  ( 4.071447262713884463, -4.041451884327383226, 0.000000000000000000 ) ) ;
#3276 = DIRECTION ( 'NONE',  ( 0.000000000000000000, 0.000000000000000000, 1.000000000000000000 ) ) ;
#3277 = LINE ( 'NONE', #1729, #17593 ) ;
#3278 = CARTESIAN_POINT ( 'NONE',  ( -7.500000000000024869, -0.9711575687493196885, 9.522727272727292913 ) ) ;
#3279 = FACE_OUTER_BOUND ( 'NONE', #6126, .T. ) ;
#3280 = CIRCLE ( 'NONE', #5528, 2.500000000000000444 ) ;
#3281 = CYLINDRICAL_SURFACE ( 'NONE', #5471, 2.549999999999998934 ) ;
#3282 = CARTESIAN_POINT ( 'NONE',  ( -3.200000000000091660, -2.000000000000043521, 7.500000000000047962 ) ) ;
#3283 = CIRCLE ( 'NONE', #4379, 2.549999999999996714 ) ;
#3284 = DIRECTION ( 'NONE',  ( 1.000000000000000000, 4.440892098500626162E-16, -5.551115123125782702E-16 ) ) ;
#3285 = LINE ( 'NONE', #4514, #2201 ) ;
#3286 = CARTESIAN_POINT ( 'NONE',  ( 124.5000000000019469, -13.52760560296373171, -2.550000000000019806 ) ) ;
#3287 = VECTOR ( 'NONE', #13225, 1000.000000000000000 ) ;
#3288 = CARTESIAN_POINT ( 'NONE',  ( 66.26395429947837101, -4.000000000000003553, -5.999999999999956479 ) ) ;
#3289 = DIRECTION ( 'NONE',  ( 5.551115123125782702E-16, 3.966469614587832056E-31, 1.000000000000000000 ) ) ;
#3290 = ORIENTED_EDGE ( 'NONE', *, *, #4682, .F. ) ;
#3291 = ORIENTED_EDGE ( 'NONE', *, *, #10387, .F. ) ;
#3292 = VECTOR ( 'NONE', #8690, 1000.000000000000000 ) ;
#3293 = DIRECTION ( 'NONE',  ( -7.860214984770699307E-18, 1.409037165336591006E-16, 1.000000000000000000 ) ) ;
#3295 = EDGE_LOOP ( 'NONE', ( #11091, #15247, #11211, #13649 ) ) ;
#3294 = ORIENTED_EDGE ( 'NONE', *, *, #5491, .T. ) ;
#3296 = AXIS2_PLACEMENT_3D ( 'NONE', #3066, #8478, #2951 ) ;
#3297 = CARTESIAN_POINT ( 'NONE',  ( 0.000000000000000000, -14.99999999999997513, -1.387778780781445676E-14 ) ) ;
#3298 = ORIENTED_EDGE ( 'NONE', *, *, #6520, .T. ) ;
#3299 = CARTESIAN_POINT ( 'NONE',  ( 3.999999999999955147, -2.309401076758532678, -0.5000000000000004441 ) ) ;
#3300 = LINE ( 'NONE', #23184, #14482 ) ;
#3301 = EDGE_CURVE ( 'NONE', #7035, #10831, #20204, .T. ) ;
#3302 = DIRECTION ( 'NONE',  ( -2.220446049250313081E-16, 1.000000000000000000, -7.025792437124636392E-31 ) ) ;
#3303 = VECTOR ( 'NONE', #8021, 1000.000000000000000 ) ;
#3304 = ORIENTED_EDGE ( 'NONE', *, *, #8695, .T. ) ;
#3305 = DIRECTION ( 'NONE',  ( -6.106226635438366889E-16, 1.000000000000000000, -1.409037165336591006E-16 ) ) ;
#3306 = CARTESIAN_POINT ( 'NONE',  ( 3.806834918298646731, -3.031088913245542749, -1.750000000000002887 ) ) ;
#3307 = DIRECTION ( 'NONE',  ( -1.927470528863118556E-16, 1.000000000000000000, -1.252855843761027101E-14 ) ) ;
#3308 = AXIS2_PLACEMENT_3D ( 'NONE', #22985, #3449, #14273 ) ;
#3309 = CARTESIAN_POINT ( 'NONE',  ( 0.3208286057739342945, -4.433571671609761289, -0.3503314178413123869 ) ) ;
#3310 = DIRECTION ( 'NONE',  ( 0.000000000000000000, 0.000000000000000000, 1.000000000000000000 ) ) ;
#3311 = VECTOR ( 'NONE', #7956, 1000.000000000000000 ) ;
#3312 = CARTESIAN_POINT ( 'NONE',  ( 4.142654963991865280, 2.035398498734349637, -3.525413613457325734 ) ) ;
#3313 = DIRECTION ( 'NONE',  ( 1.000000000000000000, 0.000000000000000000, 0.000000000000000000 ) ) ;
#3314 = LINE ( 'NONE', #17770, #5546 ) ;
#3315 = CIRCLE ( 'NONE', #2171, 0.5000000000000038858 ) ;
#3316 =( NAMED_UNIT ( * ) PLANE_ANGLE_UNIT ( ) SI_UNIT ( $, .RADIAN. ) );
#3317 = SURFACE_STYLE_USAGE ( .BOTH. , #14128 ) ;
#3318 = ORIENTED_EDGE ( 'NONE', *, *, #2199, .F. ) ;
#3319 = DIRECTION ( 'NONE',  ( 9.714451465470119729E-16, 1.334219193460661756E-15, -1.000000000000000000 ) ) ;
#3321 = VERTEX_POINT ( 'NONE', #11278 ) ;
#3320 = ORIENTED_EDGE ( 'NONE', *, *, #15580, .T. ) ;
#3322 = CIRCLE ( 'NONE', #10815, 0.5000000000000029976 ) ;
#3323 = ORIENTED_EDGE ( 'NONE', *, *, #15166, .T. ) ;
#3325 = ORIENTED_EDGE ( 'NONE', *, *, #14140, .F. ) ;
#3324 = ORIENTED_EDGE ( 'NONE', *, *, #353, .T. ) ;
#3326 = CARTESIAN_POINT ( 'NONE',  ( -5.416517661024182750, 35.99999999900385461, -25.65091751284785815 ) ) ;
#3327 = DIRECTION ( 'NONE',  ( 3.885780586188016830E-16, 4.437342591868156373E-31, -1.000000000000000000 ) ) ;
#3328 = EDGE_CURVE ( 'NONE', #21722, #16175, #10051, .T. ) ;
#3329 = DIRECTION ( 'NONE',  ( 0.000000000000000000, -7.888609052210128564E-31, 1.000000000000000000 ) ) ;
#3330 = DIRECTION ( 'NONE',  ( -1.000000000000000000, 1.550910762415566494E-16, -8.566929763922626680E-48 ) ) ;
#3331 = DIRECTION ( 'NONE',  ( -0.7071067811865490160, -0.7071067811865460184, -1.565905175853766674E-16 ) ) ;
#3332 = VECTOR ( 'NONE', #9653, 1000.000000000000000 ) ;
#3333 = CARTESIAN_POINT ( 'NONE',  ( -6.000000000000130562, 5.299999999999957190, -8.000000000000035527 ) ) ;
#3334 = CARTESIAN_POINT ( 'NONE',  ( 4.690415759823464370, -0.7499999999999383826, -2.131890305193608448 ) ) ;
#3335 = DIRECTION ( 'NONE',  ( -3.885780586188016830E-16, -4.437342591868156373E-31, 1.000000000000000000 ) ) ;
#3336 = VECTOR ( 'NONE', #22675, 1000.000000000000000 ) ;
#3337 = FACE_OUTER_BOUND ( 'NONE', #22877, .T. ) ;
#3338 = EDGE_CURVE ( 'NONE', #18645, #15739, #6230, .T. ) ;
#3339 = CARTESIAN_POINT ( 'NONE',  ( -42.54314575050793934, -4.000000000000021316, 7.500000000000062172 ) ) ;
#3340 = CIRCLE ( 'NONE', #16445, 0.4999999999999994449 ) ;
#3341 = VECTOR ( 'NONE', #7356, 1000.000000000000000 ) ;
#3342 = EDGE_CURVE ( 'NONE', #11851, #10462, #21836, .T. ) ;
#3343 = DIRECTION ( 'NONE',  ( 1.000000000000000000, 0.000000000000000000, 0.000000000000000000 ) ) ;
#3344 = DIRECTION ( 'NONE',  ( 0.000000000000000000, 6.938893903907245733E-15, 1.000000000000000000 ) ) ;
#3345 = EDGE_CURVE ( 'NONE', #13984, #18025, #2914, .T. ) ;
#3346 = CARTESIAN_POINT ( 'NONE',  ( 10.50000000000000888, -14.00000000000003020, 5.750000000000047073 ) ) ;
#3347 = DIRECTION ( 'NONE',  ( -9.121204216617949000E-31, -1.000000000000000000, 6.982962677686261977E-15 ) ) ;
#3348 = CARTESIAN_POINT ( 'NONE',  ( -3.999999999998653966, -1.658469974638416167, -3.531532913076295355 ) ) ;
#3349 = DIRECTION ( 'NONE',  ( 0.000000000000000000, 0.000000000000000000, -1.000000000000000000 ) ) ;
#3350 =( GEOMETRIC_REPRESENTATION_CONTEXT ( 3 ) GLOBAL_UNCERTAINTY_ASSIGNED_CONTEXT ( ( #13328 ) ) GLOBAL_UNIT_ASSIGNED_CONTEXT ( ( #22674, #15238, #21022 ) ) REPRESENTATION_CONTEXT ( 'NONE', 'WORKASPACE' ) );
#3351 = VERTEX_POINT ( 'NONE', #14925 ) ;
#3352 = PRODUCT_CONTEXT ( 'NONE', #7881, 'mechanical' ) ;
#3354 = ORIENTED_EDGE ( 'NONE', *, *, #20656, .T. ) ;
#3353 = EDGE_LOOP ( 'NONE', ( #11315, #3942, #1859 ) ) ;
#3355 = ORIENTED_EDGE ( 'NONE', *, *, #21250, .F. ) ;
#3356 = ADVANCED_FACE ( 'NONE', ( #20467 ), #16910, .F. ) ;
#3357 = PRESENTATION_LAYER_ASSIGNMENT (  '', '', ( #20634 ) ) ;
#3358 = EDGE_LOOP ( 'NONE', ( #20124, #21694, #4218, #3491 ) ) ;
#3359 = AXIS2_PLACEMENT_3D ( 'NONE', #4417, #20795, #1373 ) ;
#3360 = AXIS2_PLACEMENT_3D ( 'NONE', #9607, #211, #5969 ) ;
#3361 = EDGE_LOOP ( 'NONE', ( #11658, #10861, #15972, #630 ) ) ;
#3362 = ORIENTED_EDGE ( 'NONE', *, *, #15001, .F. ) ;
#3363 = DIRECTION ( 'NONE',  ( 1.000000000000000000, 5.598259082250514647E-17, 3.330669073875432643E-16 ) ) ;
#3364 = CARTESIAN_POINT ( 'NONE',  ( 0.3126073911696378160, -2.020725942163709377, 3.500000000000003109 ) ) ;
#3365 = ORIENTED_EDGE ( 'NONE', *, *, #11287, .T. ) ;
#3366 = CARTESIAN_POINT ( 'NONE',  ( -55.25320565519145788, 9.020562075079396891E-14, 10.00000000000009237 ) ) ;
#3367 = COLOUR_RGB ( '', 0.72549020, 0.75294118, 0.79215686) ;
#3368 = CARTESIAN_POINT ( 'NONE',  ( -6.938893903861184144E-14, 0.7368602791855416445, -4.750000000000013323 ) ) ;
#3369 = ADVANCED_FACE ( 'NONE', ( #22349 ), #11504, .F. ) ;
#3370 = DIRECTION ( 'NONE',  ( 0.000000000000000000, 0.000000000000000000, 1.000000000000000000 ) ) ;
#3371 = DIRECTION ( 'NONE',  ( 1.000000000000000000, 2.699383410053119644E-30, 3.330669073875432643E-16 ) ) ;
#3372 = CARTESIAN_POINT ( 'NONE',  ( -7.644579933246753001, -0.8425218428686375161, 8.321099285265791679 ) ) ;
#3373 = CARTESIAN_POINT ( 'NONE',  ( 4.000000000000003553, 1.935983797701079423, -5.350530693383767300 ) ) ;
#3374 = LINE ( 'NONE', #11937, #18273 ) ;
#3375 = EDGE_CURVE ( 'NONE', #9172, #5639, #16048, .T. ) ;
#3376 = AXIS2_PLACEMENT_3D ( 'NONE', #14373, #3673, #1682 ) ;
#3377 = DIRECTION ( 'NONE',  ( 1.000000000000000000, 1.492474417944841737E-16, 3.842941406090992613E-32 ) ) ;
#3378 = DIRECTION ( 'NONE',  ( -1.733449886265890494E-32, -4.190823558986611203E-31, 1.000000000000000000 ) ) ;
#3379 = FACE_OUTER_BOUND ( 'NONE', #16026, .T. ) ;
#3380 = ORIENTED_EDGE ( 'NONE', *, *, #10802, .T. ) ;
#3381 = DIRECTION ( 'NONE',  ( 2.775557561562883955E-17, -3.406761633869148333E-16, 1.000000000000000000 ) ) ;
#3382 = CARTESIAN_POINT ( 'NONE',  ( -4.182466315668081691, 13.41110669254460852, -29.00000000000000000 ) ) ;
#3383 = AXIS2_PLACEMENT_3D ( 'NONE', #17279, #19525, #6473 ) ;
#3385 = ORIENTED_EDGE ( 'NONE', *, *, #13961, .T. ) ;
#3384 = ORIENTED_EDGE ( 'NONE', *, *, #3742, .T. ) ;
#3386 = EDGE_CURVE ( 'NONE', #3717, #5983, #820, .T. ) ;
#3387 = EDGE_LOOP ( 'NONE', ( #14017, #3325, #21955, #10024 ) ) ;
#3388 = EDGE_LOOP ( 'NONE', ( #19454, #20353, #18890 ) ) ;
#3389 = FACE_OUTER_BOUND ( 'NONE', #19082, .T. ) ;
#3390 = LINE ( 'NONE', #17722, #12919 ) ;
#3391 = CARTESIAN_POINT ( 'NONE',  ( 7.786490775660112718, -0.7065074219475176998, 7.963863235126067863 ) ) ;
#3392 = EDGE_CURVE ( 'NONE', #22415, #9172, #17263, .T. ) ;
#3393 = CYLINDRICAL_SURFACE ( 'NONE', #12644, 0.4999999999999987232 ) ;
#3394 = CARTESIAN_POINT ( 'NONE',  ( 0.000000000000000000, 0.000000000000000000, 0.000000000000000000 ) ) ;
#3395 = CARTESIAN_POINT ( 'NONE',  ( -50.65685424949267457, -7.200000000000049916, 8.000000000000035527 ) ) ;
#3396 = CARTESIAN_POINT ( 'NONE',  ( 4.050880675075974047, 1.379097446046313902, 3.567934390854443194 ) ) ;
#3397 = CIRCLE ( 'NONE', #11268, 3.113037248396080425 ) ;
#3398 = CARTESIAN_POINT ( 'NONE',  ( -8.178874953434677408, -0.007851515978185664296, 6.644730819938938104 ) ) ;
#3399 = CARTESIAN_POINT ( 'NONE',  ( 0.000000000000000000, 11.00000000000000000, -10.86602540378443749 ) ) ;
#3400 = CARTESIAN_POINT ( 'NONE',  ( 0.000000000000000000, 0.000000000000000000, 0.000000000000000000 ) ) ;
#3401 = CARTESIAN_POINT ( 'NONE',  ( 37.46001462128847947, 10.83019807384524036, -10.46001462128798210 ) ) ;
#3402 = PLANE ( 'NONE',  #15141 ) ;
#3403 = CARTESIAN_POINT ( 'NONE',  ( -1.040834085586084257E-13, 4.862606272033151100, -3.745885042887441063 ) ) ;
#3404 = DIRECTION ( 'NONE',  ( 1.000000000000000000, -7.477632011778292156E-48, 3.885780586188017323E-16 ) ) ;
#3405 = FACE_OUTER_BOUND ( 'NONE', #18244, .T. ) ;
#3406 = VERTEX_POINT ( 'NONE', #22931 ) ;
#3407 = CIRCLE ( 'NONE', #6412, 2.550000000000010481 ) ;
#3408 = VERTEX_POINT ( 'NONE', #19047 ) ;
#3409 = B_SPLINE_CURVE_WITH_KNOTS ( 'NONE', 3,
 ( #8006, #18597, #6365, #16923, #22124 ),
 .UNSPECIFIED., .F., .F.,
 ( 4, 1, 4 ),
 ( 0.000000000000000000, 0.002309401076758508826, 0.004618802153517017652 ),
 .UNSPECIFIED. ) ;
#3411 = ORIENTED_EDGE ( 'NONE', *, *, #22441, .F. ) ;
#3410 = ORIENTED_EDGE ( 'NONE', *, *, #15391, .T. ) ;
#3412 = CARTESIAN_POINT ( 'NONE',  ( 0.5469614295417839500, -4.303013824935142395, -3.535263753545104581 ) ) ;
#3413 = ADVANCED_FACE ( 'NONE', ( #11862 ), #11529, .T. ) ;
#3414 = DIRECTION ( 'NONE',  ( 1.000000000000000000, 2.168404344970992105E-16, 0.000000000000000000 ) ) ;
#3415 = DIRECTION ( 'NONE',  ( -2.220446049250313081E-16, 1.000000000000000000, -7.025792437124636392E-31 ) ) ;
#3416 = DIRECTION ( 'NONE',  ( 0.7071067811865485719, -0.7071067811865464625, -1.010793663541191485E-16 ) ) ;
#3417 = ORIENTED_EDGE ( 'NONE', *, *, #2463, .F. ) ;
#3418 = CARTESIAN_POINT ( 'NONE',  ( -45.56568542494949980, 0.5000000000000559552, -7.500000000000007105 ) ) ;
#3419 = DIRECTION ( 'NONE',  ( 1.333893503340774882E-15, 2.778352770573747380E-17, 1.000000000000000000 ) ) ;
#3420 = LINE ( 'NONE', #8830, #19196 ) ;
#3421 = EDGE_CURVE ( 'NONE', #19136, #15368, #22699, .T. ) ;
#3422 = CARTESIAN_POINT ( 'NONE',  ( -6.999999999999992006, -13.02884243125069652, 9.522727272727321335 ) ) ;
#3423 = LINE ( 'NONE', #20, #10327 ) ;
#3424 = DIRECTION ( 'NONE',  ( -2.775557561562883647E-17, 3.652049423109057473E-16, -1.000000000000000000 ) ) ;
#3425 = VECTOR ( 'NONE', #18709, 1000.000000000000000 ) ;
#3426 = CARTESIAN_POINT ( 'NONE',  ( 2.775557561562891351E-14, 2.999999999999999112, -6.499999999999950262 ) ) ;
#3427 = CARTESIAN_POINT ( 'NONE',  ( -5.089746846163173136E-15, 5.495644160703784365E-16, 4.487534009422209813 ) ) ;
#3428 = CARTESIAN_POINT ( 'NONE',  ( 4.093692494532772841, -4.043567292011542413, 5.760878920963493723E-18 ) ) ;
#3429 = ORIENTED_EDGE ( 'NONE', *, *, #9910, .T. ) ;
#3431 = EDGE_LOOP ( 'NONE', ( #6975, #7910, #4809, #2968 ) ) ;
#3430 = ORIENTED_EDGE ( 'NONE', *, *, #19341, .F. ) ;
#3432 = ORIENTED_EDGE ( 'NONE', *, *, #18423, .T. ) ;
#3434 = ORIENTED_EDGE ( 'NONE', *, *, #745, .F. ) ;
#3433 = ORIENTED_EDGE ( 'NONE', *, *, #3838, .F. ) ;
#3435 = AXIS2_PLACEMENT_3D ( 'NONE', #2225, #7637, #17884 ) ;
#3436 = AXIS2_PLACEMENT_3D ( 'NONE', #15590, #19235, #17590 ) ;
#3437 = CARTESIAN_POINT ( 'NONE',  ( -6.590924991937371580, 35.99999999900385461, -26.24135183128864313 ) ) ;
#3438 = CARTESIAN_POINT ( 'NONE',  ( -3.499999999708153453, 13.99999999900385106, -26.00000000000000000 ) ) ;
#3439 = LINE ( 'NONE', #454, #22988 ) ;
#3440 = CARTESIAN_POINT ( 'NONE',  ( -8.697224362268011433, -12.00000000000004263, 6.250000000000019540 ) ) ;
#3441 = DIRECTION ( 'NONE',  ( 3.241725282392603095E-30, 1.000000000000000000, -2.218671295934100958E-31 ) ) ;
#3442 = DIRECTION ( 'NONE',  ( -1.066786462891689527E-26, -6.656013887802287108E-31, -1.000000000000000000 ) ) ;
#3443 = CARTESIAN_POINT ( 'NONE',  ( 12.84999999999997300, -12.00000000000006928, 4.163336342344337027E-14 ) ) ;
#3444 = DIRECTION ( 'NONE',  ( 1.454462294001240516E-30, 1.000000000000000000, 0.000000000000000000 ) ) ;
#3445 = DIRECTION ( 'NONE',  ( -1.000000000000000000, 1.409462824231139829E-14, 0.000000000000000000 ) ) ;
#3446 = DIRECTION ( 'NONE',  ( -0.000000000000000000, -0.000000000000000000, 1.000000000000000000 ) ) ;
#3447 = CARTESIAN_POINT ( 'NONE',  ( -10.49999999999999467, -12.00000000000000711, 9.250000000000021316 ) ) ;
#3448 = PRODUCT_DEFINITION ( 'UNKNOWN', '', #18771, #20179 ) ;
#3449 = DIRECTION ( 'NONE',  ( 1.000000000000000000, 1.479114197289388027E-30, -2.013525853228518840E-32 ) ) ;
#3450 = CARTESIAN_POINT ( 'NONE',  ( 7.862302507584130851, -2.046564842090945913, 6.866983975782614102 ) ) ;
#3451 = CIRCLE ( 'NONE', #16569, 3.499999999999995115 ) ;
#3452 = CARTESIAN_POINT ( 'NONE',  ( -4.203934362469490260, -1.640673743454793776, -3.598432614607018465 ) ) ;
#3453 = LINE ( 'NONE', #10390, #10772 ) ;
#3454 = ORIENTED_EDGE ( 'NONE', *, *, #4753, .F. ) ;
#3455 = EDGE_CURVE ( 'NONE', #21891, #15244, #13752, .T. ) ;
#3457 = EDGE_LOOP ( 'NONE', ( #6063, #11657, #9748, #12715 ) ) ;
#3456 = VERTEX_POINT ( 'NONE', #8333 ) ;
#3458 = ORIENTED_EDGE ( 'NONE', *, *, #20035, .T. ) ;
#3459 = EDGE_CURVE ( 'NONE', #12296, #371, #4561, .T. ) ;
#3461 = ORIENTED_EDGE ( 'NONE', *, *, #15395, .F. ) ;
#3460 = ORIENTED_EDGE ( 'NONE', *, *, #21410, .F. ) ;
#3462 = ORIENTED_EDGE ( 'NONE', *, *, #5486, .F. ) ;
#3463 = EDGE_LOOP ( 'NONE', ( #15742, #4728, #11787, #887 ) ) ;
#3464 = ORIENTED_EDGE ( 'NONE', *, *, #18747, .F. ) ;
#3465 = CARTESIAN_POINT ( 'NONE',  ( 29.00000000029184832, 16.99999999900385461, -19.49999999999998934 ) ) ;
#3466 = VECTOR ( 'NONE', #22189, 1000.000000000000000 ) ;
#3467 = CARTESIAN_POINT ( 'NONE',  ( 0.000000000000000000, 0.000000000000000000, 3.499999999999975131 ) ) ;
#3468 = DIRECTION ( 'NONE',  ( 1.000000000000000000, -4.615739097524200579E-16, -1.134196829589820086E-15 ) ) ;
#3469 = CIRCLE ( 'NONE', #11737, 6.000000000000047073 ) ;
#3470 = CARTESIAN_POINT ( 'NONE',  ( 26.09619407800442659, 29.09619407671642222, -18.50000000000000355 ) ) ;
#3471 = DIRECTION ( 'NONE',  ( -1.000000000000000000, -1.479114197289397135E-31, -5.916456789157588541E-31 ) ) ;
#3472 = CARTESIAN_POINT ( 'NONE',  ( -3.999999999708139686, 35.99999999900384751, -26.00000000000000711 ) ) ;
#3473 = FACE_OUTER_BOUND ( 'NONE', #2172, .T. ) ;
#3474 =( LENGTH_UNIT ( ) NAMED_UNIT ( * ) SI_UNIT ( .MILLI., .METRE. ) );
#3475 = EDGE_CURVE ( 'NONE', #3554, #14655, #4393, .T. ) ;
#3476 = DIRECTION ( 'NONE',  ( -2.172745813409349776E-17, 1.000000000000000000, -1.309377075419428048E-16 ) ) ;
#3477 = TOROIDAL_SURFACE ( 'NONE', #18118, 9.499999999999998224, 0.5000000000000000000 ) ;
#3478 = DIRECTION ( 'NONE',  ( 0.000000000000000000, 1.000000000000000000, 0.000000000000000000 ) ) ;
#3479 = FACE_OUTER_BOUND ( 'NONE', #7877, .T. ) ;
#3480 = VERTEX_POINT ( 'NONE', #3282 ) ;
#3481 = EDGE_CURVE ( 'NONE', #11583, #22878, #279, .T. ) ;
#3482 = FILL_AREA_STYLE_COLOUR ( '', #9353 ) ;
#3483 = CARTESIAN_POINT ( 'NONE',  ( 4.071447262713891568, -2.020725942163709377, -3.499999999999999556 ) ) ;
#3484 = FACE_OUTER_BOUND ( 'NONE', #9188, .T. ) ;
#3486 = ORIENTED_EDGE ( 'NONE', *, *, #20226, .T. ) ;
#3485 = VERTEX_POINT ( 'NONE', #11970 ) ;
#3487 = AXIS2_PLACEMENT_3D ( 'NONE', #1947, #5618, #2188 ) ;
#3488 = AXIS2_PLACEMENT_3D ( 'NONE', #3929, #18287, #2162 ) ;
#3489 = CIRCLE ( 'NONE', #12491, 3.500000000000013323 ) ;
#3490 = EDGE_CURVE ( 'NONE', #10462, #12775, #12820, .T. ) ;
#3491 = ORIENTED_EDGE ( 'NONE', *, *, #8983, .F. ) ;
#3492 = EDGE_CURVE ( 'NONE', #15314, #16729, #20217, .T. ) ;
#3493 = EDGE_LOOP ( 'NONE', ( #8371, #1521, #6300, #20864 ) ) ;
#3494 = EDGE_CURVE ( 'NONE', #2294, #19191, #2927, .T. ) ;
#3495 = FACE_OUTER_BOUND ( 'NONE', #12885, .T. ) ;
#3496 = FACE_OUTER_BOUND ( 'NONE', #2492, .T. ) ;
#3497 = DIRECTION ( 'NONE',  ( -1.734723475976813750E-16, -1.000000000000000000, 3.469446951953607484E-15 ) ) ;
#3498 = VECTOR ( 'NONE', #14349, 1000.000000000000000 ) ;
#3499 = CARTESIAN_POINT ( 'NONE',  ( -42.54314575050793934, 4.799999999999998934, 7.500000000000062172 ) ) ;
#3500 = AXIS2_PLACEMENT_3D ( 'NONE', #4714, #11883, #19065 ) ;
#3501 = CARTESIAN_POINT ( 'NONE',  ( 0.000000000000000000, -0.5999999999999894307, -4.749999999999948486 ) ) ;
#3502 = FACE_OUTER_BOUND ( 'NONE', #8907, .T. ) ;
#3503 = PRESENTATION_LAYER_ASSIGNMENT (  '', '', ( #10630 ) ) ;
#3504 = CIRCLE ( 'NONE', #1638, 2.500000000000003997 ) ;
#3505 = DIRECTION ( 'NONE',  ( 1.000000000000000000, 2.699383410053117892E-30, 3.885780586188017323E-16 ) ) ;
#3506 = ADVANCED_FACE ( 'NONE', ( #10104 ), #17377, .T. ) ;
#3507 = EDGE_CURVE ( 'NONE', #5668, #11952, #11551, .T. ) ;
#3508 = PLANE ( 'NONE',  #18983 ) ;
#3509 = EDGE_CURVE ( 'NONE', #18638, #9788, #19382, .T. ) ;
#3510 = CARTESIAN_POINT ( 'NONE',  ( 37.69160037009659447, 10.97664592903645087, -10.51717533640882962 ) ) ;
#3511 = CARTESIAN_POINT ( 'NONE',  ( 0.000000000000000000, 0.000000000000000000, 0.000000000000000000 ) ) ;
#3512 = FACE_OUTER_BOUND ( 'NONE', #14015, .T. ) ;
#3513 = CARTESIAN_POINT ( 'NONE',  ( -6.000000000000116351, -8.000000000000003553, -8.000000000000007105 ) ) ;
#3514 = CARTESIAN_POINT ( 'NONE',  ( 63.53596085922837489, -2.925414806476733798, -6.499999999999957367 ) ) ;
#3515 = ORIENTED_EDGE ( 'NONE', *, *, #2658, .F. ) ;
#3516 = EDGE_CURVE ( 'NONE', #6724, #14530, #13864, .T. ) ;
#3517 = VECTOR ( 'NONE', #15735, 1000.000000000000000 ) ;
#3518 = ADVANCED_FACE ( 'NONE', ( #18932 ), #21046, .T. ) ;
#3519 = AXIS2_PLACEMENT_3D ( 'NONE', #3751, #240, #2103 ) ;
#3520 = VERTEX_POINT ( 'NONE', #8570 ) ;
#3521 = TOROIDAL_SURFACE ( 'NONE', #15164, 5.750000000000000000, 0.5000000000000000000 ) ;
#3522 = AXIS2_PLACEMENT_3D ( 'NONE', #18916, #17130, #22443 ) ;
#3523 = EDGE_CURVE ( 'NONE', #20968, #9827, #7435, .T. ) ;
#3524 = CIRCLE ( 'NONE', #10653, 3.500000000000004441 ) ;
#3525 = CARTESIAN_POINT ( 'NONE',  ( -5.523909222203892355, 35.99999999900385461, -25.97380687558948864 ) ) ;
#3527 = VERTEX_POINT ( 'NONE', #13636 ) ;
#3526 = EDGE_LOOP ( 'NONE', ( #9450, #17571, #30, #2037 ) ) ;
#3528 = EDGE_CURVE ( 'NONE', #2913, #5438, #20588, .T. ) ;
#3529 = APPLICATION_CONTEXT ( 'automotive_design' ) ;
#3530 = DIRECTION ( 'NONE',  ( -1.000000000000000000, -2.699383410053119644E-30, -3.330669073875432643E-16 ) ) ;
#3531 = DIRECTION ( 'NONE',  ( -2.168404344970994323E-16, 1.000000000000000000, -1.577721810442023611E-30 ) ) ;
#3532 = PRESENTATION_STYLE_ASSIGNMENT (( #1410 ) ) ;
#3533 = FACE_OUTER_BOUND ( 'NONE', #11873, .T. ) ;
#3534 = ORIENTED_EDGE ( 'NONE', *, *, #817, .F. ) ;
#3535 = CARTESIAN_POINT ( 'NONE',  ( 12.49999999999992362, 1.500000000000015099, -14.49999999999999822 ) ) ;
#3536 = CARTESIAN_POINT ( 'NONE',  ( 2.775557561562891351E-14, 2.999999999999999112, -12.50000000000001066 ) ) ;
#3537 = CARTESIAN_POINT ( 'NONE',  ( 6.495190528383244732, 4.999999999999948486, -3.750000000000000000 ) ) ;
#3538 = DIRECTION ( 'NONE',  ( -0.000000000000000000, -1.000000000000000000, 0.000000000000000000 ) ) ;
#3539 = DIRECTION ( 'NONE',  ( -0.000000000000000000, 1.000000000000000000, 0.000000000000000000 ) ) ;
#3540 = AXIS2_PLACEMENT_3D ( 'NONE', #22902, #8775, #8892 ) ;
#3541 = CARTESIAN_POINT ( 'NONE',  ( 8.723547172042470876, -2.015988055643229693, 6.817515300135711165 ) ) ;
#3542 = CARTESIAN_POINT ( 'NONE',  ( -4.000000000000003553, -2.309401076758532678, -0.3572655899081733644 ) ) ;
#3543 = FACE_OUTER_BOUND ( 'NONE', #11206, .T. ) ;
#3544 = CONICAL_SURFACE ( 'NONE', #1673, 12.50000000000003375, 0.1651486774146268266 ) ;
#3545 = CARTESIAN_POINT ( 'NONE',  ( -6.000000000000019540, -5.300000000000006040, 7.500000000000062172 ) ) ;
#3546 = DIRECTION ( 'NONE',  ( -1.000000000000000000, -3.254448077276381206E-32, -1.066788928082016908E-26 ) ) ;
#3547 = ORIENTED_EDGE ( 'NONE', *, *, #5939, .F. ) ;
#3548 = APPLICATION_PROTOCOL_DEFINITION ( 'draft international standard', 'automotive_design', 1998, #22871 ) ;
#3550 = ORIENTED_EDGE ( 'NONE', *, *, #472, .T. ) ;
#3549 = ORIENTED_EDGE ( 'NONE', *, *, #4802, .F. ) ;
#3551 = EDGE_CURVE ( 'NONE', #22821, #1743, #14561, .T. ) ;
#3552 = EDGE_LOOP ( 'NONE', ( #11060, #2796, #4284, #4278 ) ) ;
#3553 = CIRCLE ( 'NONE', #12560, 2.499999999999990674 ) ;
#3555 = ORIENTED_EDGE ( 'NONE', *, *, #21049, .F. ) ;
#3554 = VERTEX_POINT ( 'NONE', #16313 ) ;
#3556 = CLOSED_SHELL ( 'NONE', ( #776, #2224, #11261, #5049, #11846, #352, #8243, #13392, #22580, #19269, #19759, #9442, #4069, #18165, #19024, #3787, #69, #9250, #19718, #16371, #5190, #12684, #10694, #5867, #641, #17883, #22382, #2309, #18646 ) ) ;
#3557 = AXIS2_PLACEMENT_3D ( 'NONE', #2340, #7414, #14926 ) ;
#3558 = CARTESIAN_POINT ( 'NONE',  ( -4.113620667976089607, -1.750000000000001554, -2.375000000000005773 ) ) ;
#3559 = DIRECTION ( 'NONE',  ( 1.734723475976805517E-15, 0.000000000000000000, 1.000000000000000000 ) ) ;
#3560 = CARTESIAN_POINT ( 'NONE',  ( 7.120027569165137571, -11.54977705885981898, 8.099087005775212234 ) ) ;
#3561 = CARTESIAN_POINT ( 'NONE',  ( -7.862302507584129074, -11.95343515790908206, 6.866983975782633642 ) ) ;
#3562 = CARTESIAN_POINT ( 'NONE',  ( 30.00000000029184832, -9.961476088449217059E-10, 0.000000000000000000 ) ) ;
#3563 =( BOUNDED_SURFACE ( )  B_SPLINE_SURFACE ( 3, 2, ( 
 ( #3684, #12736, #508 ),
 ( #21579, #7561, #16589 ),
 ( #17924, #18045, #3906 ),
 ( #4019, #18155, #7679 ),
 ( #16368, #16484, #11201 ),
 ( #12974, #18384, #5459 ),
 ( #18265, #2260, #392 ),
 ( #5572, #9441, #14849 ),
 ( #8986, #10854, #22023 ),
 ( #14726, #9329, #16250 ),
 ( #5911, #167, #12615 ),
 ( #21691, #21918, #13085 ),
 ( #1800, #2026, #270 ),
 ( #9212, #2138, #16138 ) ),
 .UNSPECIFIED., .F., .F., .T. ) 
 B_SPLINE_SURFACE_WITH_KNOTS ( ( 4, 2, 2, 2, 2, 2, 4 ),
 ( 3, 3 ),
 ( -2.168404344971008868E-19, 0.0009385527998839222766, 0.001407829199825883469, 0.001877105599767844770, 0.002346381999709806071, 0.002815658399651766938, 0.003754211199535689540 ),
 ( 0.000000000000000000, 1.000000000000000000 ),
 .UNSPECIFIED. ) 
 GEOMETRIC_REPRESENTATION_ITEM ( )  RATIONAL_B_SPLINE_SURFACE ( (
 ( 1.000000000000000000, 0.7071067811865494601, 1.000000000000000000),
 ( 1.000000000000000000, 0.7217349950159032135, 1.000000000000000000),
 ( 1.000000000000000000, 0.7325631490737081197, 1.000000000000000000),
 ( 1.000000000000000000, 0.7426392126583249986, 1.000000000000000000),
 ( 1.000000000000000000, 0.7449451721693722828, 1.000000000000000000),
 ( 1.000000000000000000, 0.7474053618998901527, 1.000000000000000000),
 ( 1.000000000000000000, 0.7475947887410621107, 1.000000000000000000),
 ( 1.000000000000000000, 0.7461109904165270645, 1.000000000000000000),
 ( 1.000000000000000000, 0.7444113185333118832, 1.000000000000000000),
 ( 1.000000000000000000, 0.7395217850810087423, 1.000000000000000000),
 ( 1.000000000000000000, 0.7363545993504165832, 1.000000000000000000),
 ( 1.000000000000000000, 0.7253814056385120557, 1.000000000000000000),
 ( 1.000000000000000000, 0.7159765610437058836, 1.000000000000000000),
 ( 1.000000000000000000, 0.7071067811865503483, 1.000000000000000000) ) ) 
 REPRESENTATION_ITEM ( '' )  SURFACE ( )  );
#3564 = CARTESIAN_POINT ( 'NONE',  ( 7.980290731945721916, -13.39170085596636461, 7.616182555102830598 ) ) ;
#3565 = CARTESIAN_POINT ( 'NONE',  ( -55.25320565519140104, -2.700000000000049472, 10.00000000000007816 ) ) ;
#3566 = CYLINDRICAL_SURFACE ( 'NONE', #7319, 4.750000000000013323 ) ;
#3567 = CARTESIAN_POINT ( 'NONE',  ( 2.081668171172168513E-14, 10.00000000000000533, 0.000000000000000000 ) ) ;
#3568 = LINE ( 'NONE', #7214, #5792 ) ;
#3569 = DIRECTION ( 'NONE',  ( -0.000000000000000000, -0.000000000000000000, 1.000000000000000000 ) ) ;
#3570 = DIRECTION ( 'NONE',  ( 0.000000000000000000, 0.000000000000000000, 1.000000000000000000 ) ) ;
#3571 = ADVANCED_BREP_SHAPE_REPRESENTATION ( '', ( #21090, #22115 ), #13848 ) ;
#3572 = DIRECTION ( 'NONE',  ( -1.000000000000000000, -1.910522504832140594E-31, 5.551115123125818447E-17 ) ) ;
#3573 = DIRECTION ( 'NONE',  ( 1.000000000000000000, 2.168404344970995063E-16, 0.000000000000000000 ) ) ;
#3574 = CARTESIAN_POINT ( 'NONE',  ( 3.880206590543184841, -3.396506438958554863, 1.117078279488939785 ) ) ;
#3575 = ORIENTED_EDGE ( 'NONE', *, *, #7959, .F. ) ;
#3576 = SURFACE_STYLE_FILL_AREA ( #19693 ) ;
#3578 = ORIENTED_EDGE ( 'NONE', *, *, #18112, .F. ) ;
#3577 = ORIENTED_EDGE ( 'NONE', *, *, #1199, .F. ) ;
#3579 = VERTEX_POINT ( 'NONE', #8918 ) ;
#3581 = ORIENTED_EDGE ( 'NONE', *, *, #21643, .T. ) ;
#3580 = VERTEX_POINT ( 'NONE', #12316 ) ;
#3582 = B_SPLINE_CURVE_WITH_KNOTS ( 'NONE', 3,
 ( #21825, #12995, #533, #14641, #9584, #20172 ),
 .UNSPECIFIED., .F., .F.,
 ( 4, 2, 4 ),
 ( 0.001997790247439712105, 0.003382245507025886423, 0.004766700766612060741 ),
 .UNSPECIFIED. ) ;
#3583 = ORIENTED_EDGE ( 'NONE', *, *, #7960, .F. ) ;
#3584 = ORIENTED_EDGE ( 'NONE', *, *, #611, .F. ) ;
#3585 = ORIENTED_EDGE ( 'NONE', *, *, #18079, .F. ) ;
#3586 = CARTESIAN_POINT ( 'NONE',  ( 4.000000000000003553, 0.3904826640788058856, -2.016361930938861168E-15 ) ) ;
#3587 = AXIS2_PLACEMENT_3D ( 'NONE', #3044, #8332, #6580 ) ;
#3588 = AXIS2_PLACEMENT_3D ( 'NONE', #9889, #6128, #13305 ) ;
#3589 = PLANE ( 'NONE',  #2758 ) ;
#3590 = DIRECTION ( 'NONE',  ( -1.000000000000000000, 0.000000000000000000, 0.000000000000000000 ) ) ;
#3591 = DIRECTION ( 'NONE',  ( 3.885780586188016830E-16, 4.437342591868156373E-31, -1.000000000000000000 ) ) ;
#3592 = EDGE_CURVE ( 'NONE', #17679, #14402, #9311, .T. ) ;
#3593 = CARTESIAN_POINT ( 'NONE',  ( 2.775557561562891351E-14, 0.5000000000000004441, -2.133974596215532316 ) ) ;
#3594 = DIRECTION ( 'NONE',  ( 0.000000000000000000, 3.382522293539642681E-32, 1.000000000000000000 ) ) ;
#3595 = CARTESIAN_POINT ( 'NONE',  ( -6.000000000000143885, -2.000000000000043521, 8.000000000000062172 ) ) ;
#3596 = CARTESIAN_POINT ( 'NONE',  ( 3.061616997868385113E-16, 1.750000000000001554, 2.500000000000000000 ) ) ;
#3597 = DIRECTION ( 'NONE',  ( -1.000000000000000000, 0.000000000000000000, 0.000000000000000000 ) ) ;
#3598 = FACE_OUTER_BOUND ( 'NONE', #9574, .T. ) ;
#3599 = CARTESIAN_POINT ( 'NONE',  ( -50.65685424949274562, -2.700000000000125855, 7.500000000000076383 ) ) ;
#3600 = ORIENTED_EDGE ( 'NONE', *, *, #17872, .F. ) ;
#3601 = FACE_OUTER_BOUND ( 'NONE', #15852, .T. ) ;
#3602 = CARTESIAN_POINT ( 'NONE',  ( 12.84999999999997300, -1.500000000000001332, 6.250000000000005329 ) ) ;
#3604 = ORIENTED_EDGE ( 'NONE', *, *, #811, .T. ) ;
#3603 = ORIENTED_EDGE ( 'NONE', *, *, #6089, .F. ) ;
#3605 = ADVANCED_FACE ( 'NONE', ( #7165 ), #14093, .T. ) ;
#3606 = AXIS2_PLACEMENT_3D ( 'NONE', #14709, #11412, #2358 ) ;
#3607 = ORIENTED_EDGE ( 'NONE', *, *, #1466, .F. ) ;
#3608 = ORIENTED_EDGE ( 'NONE', *, *, #5772, .T. ) ;
#3609 = AXIS2_PLACEMENT_3D ( 'NONE', #2203, #3843, #13256 ) ;
#3610 = EDGE_CURVE ( 'NONE', #21919, #9975, #18693, .T. ) ;
#3611 = DIRECTION ( 'NONE',  ( 1.000000000000000000, 0.000000000000000000, 0.000000000000000000 ) ) ;
#3612 = CARTESIAN_POINT ( 'NONE',  ( 2.000000000000015543, -3.464101615137746837, 0.000000000000000000 ) ) ;
#3613 = PLANE ( 'NONE',  #13407 ) ;
#3614 = CARTESIAN_POINT ( 'NONE',  ( 3.972709601346601449, -3.429395227388333023, -1.191688283765310885 ) ) ;
#3615 = EDGE_CURVE ( 'NONE', #10242, #15995, #2169, .T. ) ;
#3616 = DIRECTION ( 'NONE',  ( 3.885780586188016830E-16, 4.437342591868156373E-31, -1.000000000000000000 ) ) ;
#3617 = CIRCLE ( 'NONE', #14510, 3.113037248396080425 ) ;
#3618 = FACE_OUTER_BOUND ( 'NONE', #4252, .T. ) ;
#3619 = DIRECTION ( 'NONE',  ( 3.885780586188016830E-16, 4.437342591868156373E-31, -1.000000000000000000 ) ) ;
#3620 = FACE_OUTER_BOUND ( 'NONE', #15096, .T. ) ;
#3621 = CARTESIAN_POINT ( 'NONE',  ( 2.918498775983380256E-10, 2.999999999003851503, 0.000000000000000000 ) ) ;
#3622 = CARTESIAN_POINT ( 'NONE',  ( 37.69139372032788771, 10.99999999999996625, -10.77870956205603648 ) ) ;
#3623 = ADVANCED_FACE ( 'NONE', ( #21741 ), #11747, .F. ) ;
#3624 = CIRCLE ( 'NONE', #16748, 2.549999999999996714 ) ;
#3625 = EDGE_CURVE ( 'NONE', #21208, #9368, #2935, .T. ) ;
#3626 = DIRECTION ( 'NONE',  ( -0.000000000000000000, -0.000000000000000000, 1.000000000000000000 ) ) ;
#3627 = DIRECTION ( 'NONE',  ( -1.000000000000000000, 0.000000000000000000, 0.000000000000000000 ) ) ;
#3629 = EDGE_CURVE ( 'NONE', #12443, #7223, #21634, .T. ) ;
#3628 = CARTESIAN_POINT ( 'NONE',  ( 0.02448733951232850634, 4.877042772274765348, -3.751161874094034232 ) ) ;
#3630 = AXIS2_PLACEMENT_3D ( 'NONE', #21717, #9123, #16284 ) ;
#3631 = FACE_OUTER_BOUND ( 'NONE', #6559, .T. ) ;
#3632 = FACE_BOUND ( 'NONE', #11089, .T. ) ;
#3633 = VERTEX_POINT ( 'NONE', #1512 ) ;
#3634 = VERTEX_POINT ( 'NONE', #12666 ) ;
#3635 = DIRECTION ( 'NONE',  ( -7.395570986446975166E-31, -3.382522293539642681E-32, -1.000000000000000000 ) ) ;
#3636 = ADVANCED_FACE ( 'NONE', ( #8685 ), #14217, .F. ) ;
#3637 = ORIENTED_EDGE ( 'NONE', *, *, #3342, .T. ) ;
#3638 = B_SPLINE_CURVE_WITH_KNOTS ( 'NONE', 3,
 ( #8768, #14522, #17945, #17833, #1711, #293 ),
 .UNSPECIFIED., .F., .F.,
 ( 4, 2, 4 ),
 ( 0.002452478801916411870, 0.003676905084148028666, 0.004901331366379645463 ),
 .UNSPECIFIED. ) ;
#3639 = CARTESIAN_POINT ( 'NONE',  ( -2.742413778650615086, 1.325747111984059590, -4.750000000000000888 ) ) ;
#3640 = DIRECTION ( 'NONE',  ( 1.333893503340774882E-15, 2.778352770573747380E-17, 1.000000000000000000 ) ) ;
#3641 = CARTESIAN_POINT ( 'NONE',  ( 4.180345304246205984, -4.135116856707421462, 0.02129519942685456982 ) ) ;
#3642 = AXIS2_PLACEMENT_3D ( 'NONE', #12147, #21464, #23116 ) ;
#3643 = VERTEX_POINT ( 'NONE', #1954 ) ;
#3644 = CARTESIAN_POINT ( 'NONE',  ( 4.690415759823415520, 0.7500000000000770495, -1.500000000000001332 ) ) ;
#3645 = CARTESIAN_POINT ( 'NONE',  ( 0.1419055191998256638, 0.6000000000000126343, -3.724211676661837167 ) ) ;
#3646 = EDGE_CURVE ( 'NONE', #15424, #18871, #5626, .T. ) ;
#3647 = CARTESIAN_POINT ( 'NONE',  ( -6.000000000000143885, -2.000000000000043521, 8.000000000000062172 ) ) ;
#3648 = CARTESIAN_POINT ( 'NONE',  ( -43.10883117545713361, -5.300000000000020250, 8.000000000000035527 ) ) ;
#3649 = DIRECTION ( 'NONE',  ( -1.000000000000000000, 1.550910762415521134E-16, -6.938893903907184004E-16 ) ) ;
#3650 = CARTESIAN_POINT ( 'NONE',  ( 42.00000000000020606, 8.000000000000003553, -0.4999999999999449329 ) ) ;
#3651 = EDGE_CURVE ( 'NONE', #19572, #18888, #18212, .T. ) ;
#3652 = CARTESIAN_POINT ( 'NONE',  ( 4.093692494532771065, 2.021783646005777424, -3.501831996793832502 ) ) ;
#3653 = ADVANCED_FACE ( 'NONE', ( #14666 ), #12306, .T. ) ;
#3654 = CARTESIAN_POINT ( 'NONE',  ( 112.6756160111033722, -11.28140466348817661, 6.500000000000088818 ) ) ;
#3655 = EDGE_LOOP ( 'NONE', ( #11959, #302 ) ) ;
#3656 = AXIS2_PLACEMENT_3D ( 'NONE', #18665, #6086, #9736 ) ;
#3657 = PRESENTATION_LAYER_ASSIGNMENT (  '', '', ( #13799 ) ) ;
#3658 = APPLICATION_PROTOCOL_DEFINITION ( 'draft international standard', 'automotive_design', 1998, #2628 ) ;
#3660 = EDGE_LOOP ( 'NONE', ( #2390, #3354, #5229, #4788 ) ) ;
#3659 = EDGE_LOOP ( 'NONE', ( #7424, #4140, #168, #20300, #7938, #21930 ) ) ;
#3661 = CIRCLE ( 'NONE', #22437, 0.5000000000000028866 ) ;
#3663 = ORIENTED_EDGE ( 'NONE', *, *, #4894, .F. ) ;
#3662 = ORIENTED_EDGE ( 'NONE', *, *, #15275, .F. ) ;
#3664 = CARTESIAN_POINT ( 'NONE',  ( -42.54314575050793934, 7.499999999999992895, -7.500000000000062172 ) ) ;
#3665 = FACE_OUTER_BOUND ( 'NONE', #8208, .T. ) ;
#3666 = CARTESIAN_POINT ( 'NONE',  ( 7.734741761309930297, -11.93000978614839269, 7.004299047562712488 ) ) ;
#3667 = DIRECTION ( 'NONE',  ( 0.7071067811865457964, -0.7071067811865492381, 0.000000000000000000 ) ) ;
#3668 = CIRCLE ( 'NONE', #22445, 0.8000000000000090372 ) ;
#3669 = ADVANCED_FACE ( 'NONE', ( #9731 ), #5739, .T. ) ;
#3670 = DIRECTION ( 'NONE',  ( -1.000000000000000000, -3.254448077276381206E-32, -1.066788928082016908E-26 ) ) ;
#3671 = FACE_BOUND ( 'NONE', #20070, .T. ) ;
#3672 = AXIS2_PLACEMENT_3D ( 'NONE', #6748, #1567, #10507 ) ;
#3673 = DIRECTION ( 'NONE',  ( 1.000000000000000000, 1.133987551255197989E-30, 1.404432126150814977E-14 ) ) ;
#3674 = DIRECTION ( 'NONE',  ( 1.333893503340774882E-15, 2.778352770573747380E-17, 1.000000000000000000 ) ) ;
#3675 = PLANE ( 'NONE',  #890 ) ;
#3676 = B_SPLINE_CURVE_WITH_KNOTS ( 'NONE', 3,
 ( #4679, #8449, #13506, #17363 ),
 .UNSPECIFIED., .F., .F.,
 ( 4, 4 ),
 ( 2.380737582390371584E-07, 0.002336974151641598059 ),
 .UNSPECIFIED. ) ;
#3677 = CARTESIAN_POINT ( 'NONE',  ( 2.775557561562891351E-14, 5.500000000000001776, -15.49999999999998579 ) ) ;
#3678 = CIRCLE ( 'NONE', #19073, 9.000000000000031974 ) ;
#3679 = CARTESIAN_POINT ( 'NONE',  ( 86.31951208941929110, -13.14189171599983119, 6.000000000000109246 ) ) ;
#3680 = EDGE_CURVE ( 'NONE', #17683, #23243, #6082, .T. ) ;
#3681 = DIRECTION ( 'NONE',  ( 1.144237745221811361E-17, -1.000000000000000000, 7.025792437124636392E-31 ) ) ;
#3682 = CARTESIAN_POINT ( 'NONE',  ( 111.0000000000017764, -13.52760560296359316, 6.500000000000068390 ) ) ;
#3683 = CARTESIAN_POINT ( 'NONE',  ( -4.773379239211084979, 35.99999999900385461, -19.50000000000000000 ) ) ;
#3684 = CARTESIAN_POINT ( 'NONE',  ( 7.500000000000007105, -1.390227771353540698, 9.250000000000019540 ) ) ;
#3685 = ORIENTED_EDGE ( 'NONE', *, *, #12395, .F. ) ;
#3687 = EDGE_LOOP ( 'NONE', ( #6041, #1746, #4892, #16938 ) ) ;
#3686 = EDGE_LOOP ( 'NONE', ( #21000, #8639, #12506 ) ) ;
#3688 = CIRCLE ( 'NONE', #22842, 5.000000000000000888 ) ;
#3689 = VERTEX_POINT ( 'NONE', #2428 ) ;
#3691 = ORIENTED_EDGE ( 'NONE', *, *, #9989, .T. ) ;
#3690 = ORIENTED_EDGE ( 'NONE', *, *, #8234, .T. ) ;
#3692 = ORIENTED_EDGE ( 'NONE', *, *, #13223, .F. ) ;
#3693 = ORIENTED_EDGE ( 'NONE', *, *, #14747, .F. ) ;
#3694 = ORIENTED_EDGE ( 'NONE', *, *, #2933, .T. ) ;
#3695 = CARTESIAN_POINT ( 'NONE',  ( 0.000000000000000000, 0.6000000000000137446, 3.054668707061600319 ) ) ;
#3696 = CIRCLE ( 'NONE', #16820, 6.000000000000023093 ) ;
#3697 = CARTESIAN_POINT ( 'NONE',  ( 1.477270212546007475E-14, -24.99999999999998224, -7.882182279042408979 ) ) ;
#3698 = ADVANCED_FACE ( 'NONE', ( #20551 ), #12911, .T. ) ;
#3699 = CARTESIAN_POINT ( 'NONE',  ( 0.000000000000000000, 0.000000000000000000, 0.000000000000000000 ) ) ;
#3700 = DIRECTION ( 'NONE',  ( -5.551115123561405253E-17, -1.000000000000000000, -2.256980353643891447E-27 ) ) ;
#3701 = CARTESIAN_POINT ( 'NONE',  ( 4.114405500665258231, -2.025575754679721729, -3.508400121684964290 ) ) ;
#3702 = DIRECTION ( 'NONE',  ( -0.000000000000000000, -1.000000000000000000, -0.000000000000000000 ) ) ;
#3703 = CARTESIAN_POINT ( 'NONE',  ( 110.9706201109471522, -13.02760560296367665, 6.000000000000088818 ) ) ;
#3704 = EDGE_CURVE ( 'NONE', #11087, #20601, #20438, .T. ) ;
#3705 = DIRECTION ( 'NONE',  ( -6.938893903907264665E-15, 1.000000000000000000, 7.642090019328551865E-31 ) ) ;
#3706 = DIRECTION ( 'NONE',  ( -3.070652698126927723E-17, -1.000000000000000000, 4.167305704548413124E-17 ) ) ;
#3707 = CARTESIAN_POINT ( 'NONE',  ( -3.200000000000133404, -2.000000000000008882, -8.000000000000035527 ) ) ;
#3708 = ORIENTED_EDGE ( 'NONE', *, *, #19543, .F. ) ;
#3709 = UNCERTAINTY_MEASURE_WITH_UNIT (LENGTH_MEASURE( 1.000000000000000082E-05 ), #13921, 'distance_accuracy_value', 'NONE');
#3710 = AXIS2_PLACEMENT_3D ( 'NONE', #19387, #21284, #3404 ) ;
#3711 = VECTOR ( 'NONE', #20089, 1000.000000000000000 ) ;
#3712 = FACE_OUTER_BOUND ( 'NONE', #1331, .T. ) ;
#3714 = ORIENTED_EDGE ( 'NONE', *, *, #8110, .F. ) ;
#3713 = ORIENTED_EDGE ( 'NONE', *, *, #617, .T. ) ;
#3715 = ADVANCED_FACE ( 'NONE', ( #22319 ), #13372, .F. ) ;
#3716 = ORIENTED_EDGE ( 'NONE', *, *, #20136, .T. ) ;
#3717 = VERTEX_POINT ( 'NONE', #2079 ) ;
#3718 = LINE ( 'NONE', #5852, #11031 ) ;
#3719 = CARTESIAN_POINT ( 'NONE',  ( -6.000000000000088818, -2.000000000000050182, -17.72029585817572084 ) ) ;
#3720 = CARTESIAN_POINT ( 'NONE',  ( -42.54314575050782565, -4.800000000000037126, -8.000000000000007105 ) ) ;
#3721 = CARTESIAN_POINT ( 'NONE',  ( 124.5000000000017195, -4.000000000000058620, 2.550000000000026468 ) ) ;
#3722 = CARTESIAN_POINT ( 'NONE',  ( -1.144235203016779945, -3.958177651039131550, -0.09382832055450740505 ) ) ;
#3723 = CARTESIAN_POINT ( 'NONE',  ( 3.973110223768726801, 0.6864646529411468912, 3.565797985667434222 ) ) ;
#3724 = LINE ( 'NONE', #7162, #17320 ) ;
#3725 = CARTESIAN_POINT ( 'NONE',  ( -4.550510256924974684, 36.49999999900384751, -19.00000000000000355 ) ) ;
#3726 = CARTESIAN_POINT ( 'NONE',  ( -67.40537636629476026, -2.700000000000125855, 12.70639812373640432 ) ) ;
#3727 = DIRECTION ( 'NONE',  ( -1.550910762415566494E-16, -1.000000000000000000, 8.135128085091684243E-31 ) ) ;
#3728 =( GEOMETRIC_REPRESENTATION_CONTEXT ( 3 ) GLOBAL_UNCERTAINTY_ASSIGNED_CONTEXT ( ( #4363 ) ) GLOBAL_UNIT_ASSIGNED_CONTEXT ( ( #14466, #7067, #15977 ) ) REPRESENTATION_CONTEXT ( 'NONE', 'WORKASPACE' ) );
#3729 = DIRECTION ( 'NONE',  ( -9.121204216617949000E-31, -1.000000000000000000, 6.982962677686261977E-15 ) ) ;
#3730 = CARTESIAN_POINT ( 'NONE',  ( 108.2426266706970637, -13.52760560296348302, 6.500000000000019540 ) ) ;
#3731 = CARTESIAN_POINT ( 'NONE',  ( -12.85000000000001386, -13.50000000000007105, 5.551115123125782702E-14 ) ) ;
#3732 = DIRECTION ( 'NONE',  ( -1.000000000000000000, -3.254448077276381206E-32, -1.066788928082016908E-26 ) ) ;
#3733 = DIRECTION ( 'NONE',  ( -0.8660254037844385966, -7.888609052210117178E-31, -0.5000000000000001110 ) ) ;
#3734 = EDGE_LOOP ( 'NONE', ( #13710, #6065, #7263, #5551 ) ) ;
#3735 = EDGE_CURVE ( 'NONE', #405, #22849, #13493, .T. ) ;
#3736 = ORIENTED_EDGE ( 'NONE', *, *, #9240, .T. ) ;
#3737 = DIRECTION ( 'NONE',  ( 0.000000000000000000, 6.938893903907237055E-15, 1.000000000000000000 ) ) ;
#3738 = DIRECTION ( 'NONE',  ( 1.333893503340774882E-15, 2.778352770573747380E-17, 1.000000000000000000 ) ) ;
#3740 = EDGE_CURVE ( 'NONE', #9641, #93, #4077, .T. ) ;
#3739 = ORIENTED_EDGE ( 'NONE', *, *, #18079, .T. ) ;
#3741 = CARTESIAN_POINT ( 'NONE',  ( 12.84999999999997300, -1.500000000000001332, -6.249999999999977796 ) ) ;
#3742 = EDGE_CURVE ( 'NONE', #16003, #3791, #13390, .T. ) ;
#3743 = LINE ( 'NONE', #15855, #4704 ) ;
#3744 = PRODUCT_DEFINITION_FORMATION_WITH_SPECIFIED_SOURCE ( 'ANY', '', #23234, .NOT_KNOWN. ) ;
#3745 = CARTESIAN_POINT ( 'NONE',  ( 4.158921614371315911, -4.076055977742331748, 0.05993604794446181355 ) ) ;
#3746 = PRESENTATION_STYLE_ASSIGNMENT (( #5292 ) ) ;
#3747 = ORIENTED_EDGE ( 'NONE', *, *, #22340, .T. ) ;
#3748 = FACE_OUTER_BOUND ( 'NONE', #15860, .T. ) ;
#3749 = DIRECTION ( 'NONE',  ( -1.000000000000000000, 0.000000000000000000, -3.717264591378832268E-16 ) ) ;
#3750 = DIRECTION ( 'NONE',  ( 0.000000000000000000, -1.000000000000000000, 0.000000000000000000 ) ) ;
#3751 = CARTESIAN_POINT ( 'NONE',  ( -6.000000000000088818, -2.000000000000043521, -7.500000000000007105 ) ) ;
#3752 = CARTESIAN_POINT ( 'NONE',  ( 7.742458795615099199, -13.26006887186488292, 8.061568688626010726 ) ) ;
#3753 = FACE_OUTER_BOUND ( 'NONE', #18820, .T. ) ;
#3754 = CARTESIAN_POINT ( 'NONE',  ( 4.154306624730736530, -2.398490048085659243, -3.721999068284422840 ) ) ;
#3755 = CARTESIAN_POINT ( 'NONE',  ( 4.086262629614036079, -4.082406995610011080, -0.07093633357111590876 ) ) ;
#3756 = LINE ( 'NONE', #8837, #14917 ) ;
#3757 = EDGE_CURVE ( 'NONE', #13088, #2421, #11135, .T. ) ;
#3758 = DIRECTION ( 'NONE',  ( -1.000000000000000000, 1.734723475976796001E-16, 0.000000000000000000 ) ) ;
#3759 = AXIS2_PLACEMENT_3D ( 'NONE', #14371, #14710, #16235 ) ;
#3760 = ORIENTED_EDGE ( 'NONE', *, *, #18965, .F. ) ;
#3761 = EDGE_CURVE ( 'NONE', #2382, #22002, #18431, .T. ) ;
#3762 = PRODUCT_CONTEXT ( 'NONE', #14336, 'mechanical' ) ;
#3764 = ORIENTED_EDGE ( 'NONE', *, *, #16718, .T. ) ;
#3763 = VERTEX_POINT ( 'NONE', #564 ) ;
#3767 = ORIENTED_EDGE ( 'NONE', *, *, #12537, .F. ) ;
#3766 = EDGE_CURVE ( 'NONE', #10170, #12123, #7498, .T. ) ;
#3765 = ORIENTED_EDGE ( 'NONE', *, *, #12267, .T. ) ;
#3768 = ADVANCED_FACE ( 'NONE', ( #14897 ), #5975, .T. ) ;
#3769 = CARTESIAN_POINT ( 'NONE',  ( -4.990285246489960080, 35.99999999900384751, -25.53533449053936621 ) ) ;
#3770 = ADVANCED_FACE ( 'NONE', ( #4182 ), #9611, .F. ) ;
#3771 = DIRECTION ( 'NONE',  ( -7.395570986446975166E-31, -3.382522293539642681E-32, -1.000000000000000000 ) ) ;
#3772 = CARTESIAN_POINT ( 'NONE',  ( 7.467942433933819402, -11.84606835491525878, 7.356484134531164898 ) ) ;
#3773 = AXIS2_PLACEMENT_3D ( 'NONE', #17, #18005, #7303 ) ;
#3774 = CARTESIAN_POINT ( 'NONE',  ( -7.026577802269679651, -11.35109376985337981, 8.453373545151620760 ) ) ;
#3775 = DIRECTION ( 'NONE',  ( -3.070652698126927723E-17, -1.000000000000000000, 4.167305704548413124E-17 ) ) ;
#3776 = DIRECTION ( 'NONE',  ( -0.000000000000000000, -0.000000000000000000, 1.000000000000000000 ) ) ;
#3777 = PRESENTATION_STYLE_ASSIGNMENT (( #7328 ) ) ;
#3778 = DIRECTION ( 'NONE',  ( 1.000000000000000000, 0.000000000000000000, -0.000000000000000000 ) ) ;
#3779 = DIRECTION ( 'NONE',  ( 1.000000000000000000, 0.000000000000000000, 0.000000000000000000 ) ) ;
#3780 = CARTESIAN_POINT ( 'NONE',  ( 4.000000000000003553, 0.3904826640788060521, -5.599999999999997868 ) ) ;
#3781 = CARTESIAN_POINT ( 'NONE',  ( 3.999999999999955147, -2.309401076758539784, -5.000000000000000888 ) ) ;
#3782 = ADVANCED_FACE ( 'NONE', ( #8074, #2661, #6554 ), #18900, .F. ) ;
#3783 = FACE_OUTER_BOUND ( 'NONE', #22504, .T. ) ;
#3784 = ADVANCED_FACE ( 'NONE', ( #22901, #9841, #4770 ), #13941, .T. ) ;
#3786 = EDGE_CURVE ( 'NONE', #12541, #21020, #15305, .T. ) ;
#3785 = DIRECTION ( 'NONE',  ( 0.000000000000000000, 0.000000000000000000, 1.000000000000000000 ) ) ;
#3787 = ADVANCED_FACE ( 'NONE', ( #15471 ), #12729, .T. ) ;
#3788 = FACE_OUTER_BOUND ( 'NONE', #18046, .T. ) ;
#3789 = CARTESIAN_POINT ( 'NONE',  ( 26.45000000029184051, 16.99999999900385461, -26.00000000000000000 ) ) ;
#3790 = CARTESIAN_POINT ( 'NONE',  ( 0.3126073911696447549, 4.041451884327383226, 0.000000000000000000 ) ) ;
#3791 = VERTEX_POINT ( 'NONE', #6319 ) ;
#3792 = AXIS2_PLACEMENT_3D ( 'NONE', #100, #212, #11012 ) ;
#3793 = AXIS2_PLACEMENT_3D ( 'NONE', #22195, #11475, #13490 ) ;
#3795 = ORIENTED_EDGE ( 'NONE', *, *, #20235, .T. ) ;
#3794 = ORIENTED_EDGE ( 'NONE', *, *, #4921, .T. ) ;
#3796 = EDGE_CURVE ( 'NONE', #12394, #7255, #8541, .T. ) ;
#3797 = EDGE_LOOP ( 'NONE', ( #17358, #22679, #6385, #5162 ) ) ;
#3800 = EDGE_LOOP ( 'NONE', ( #10927, #16895, #13953, #20041 ) ) ;
#3799 = ADVANCED_FACE ( 'NONE', ( #15232 ), #17348, .T. ) ;
#3798 = ORIENTED_EDGE ( 'NONE', *, *, #4187, .T. ) ;
#3801 = B_SPLINE_CURVE_WITH_KNOTS ( 'NONE', 3,
 ( #14316, #10551, #21036, #3612 ),
 .UNSPECIFIED., .F., .F.,
 ( 4, 4 ),
 ( 2.380737581852354520E-07, 0.002336974151641521731 ),
 .UNSPECIFIED. ) ;
#3802 = ORIENTED_EDGE ( 'NONE', *, *, #19762, .F. ) ;
#3803 = DIRECTION ( 'NONE',  ( -9.121204216617949000E-31, -1.000000000000000000, 6.982962677686261977E-15 ) ) ;
#3804 = ORIENTED_EDGE ( 'NONE', *, *, #20917, .F. ) ;
#3805 = ORIENTED_EDGE ( 'NONE', *, *, #144, .T. ) ;
#3806 = CARTESIAN_POINT ( 'NONE',  ( 0.1429064800269952973, 0.6000000000000133005, 3.726828488909540216 ) ) ;
#3807 = CARTESIAN_POINT ( 'NONE',  ( -6.938893903907228378E-15, -2.775557561562891351E-14, -7.500000000000000000 ) ) ;
#3808 = CARTESIAN_POINT ( 'NONE',  ( -42.54314575050799618, 7.499999999999992895, 8.000000000000035527 ) ) ;
#3809 = FACE_BOUND ( 'NONE', #1649, .T. ) ;
#3810 = DIRECTION ( 'NONE',  ( 2.775557561562831570E-17, 0.000000000000000000, 1.000000000000000000 ) ) ;
#3811 = AXIS2_PLACEMENT_3D ( 'NONE', #14894, #4178, #20205 ) ;
#3812 = VECTOR ( 'NONE', #13907, 1000.000000000000000 ) ;
#3813 = LINE ( 'NONE', #12404, #12902 ) ;
#3814 = CARTESIAN_POINT ( 'NONE',  ( 88.75737332930586376, -11.02760560296348125, 6.000000000000165201 ) ) ;
#3815 = DIRECTION ( 'NONE',  ( 0.000000000000000000, 0.000000000000000000, 1.000000000000000000 ) ) ;
#3816 = FACE_OUTER_BOUND ( 'NONE', #8321, .T. ) ;
#3817 = ORIENTED_EDGE ( 'NONE', *, *, #20792, .T. ) ;
#3818 = DIRECTION ( 'NONE',  ( 5.551115123561405253E-17, 1.000000000000000000, -5.963788443470795439E-28 ) ) ;
#3820 = ORIENTED_EDGE ( 'NONE', *, *, #18929, .T. ) ;
#3819 = ORIENTED_EDGE ( 'NONE', *, *, #11690, .F. ) ;
#3821 = ORIENTED_EDGE ( 'NONE', *, *, #3936, .T. ) ;
#3822 = ORIENTED_EDGE ( 'NONE', *, *, #13750, .F. ) ;
#3823 = AXIS2_PLACEMENT_3D ( 'NONE', #7895, #18714, #11645 ) ;
#3824 = CIRCLE ( 'NONE', #14357, 3.000000000000011102 ) ;
#3825 = ORIENTED_EDGE ( 'NONE', *, *, #9739, .T. ) ;
#3826 = ORIENTED_EDGE ( 'NONE', *, *, #6550, .F. ) ;
#3827 = EDGE_CURVE ( 'NONE', #21586, #749, #19124, .T. ) ;
#3828 = DIRECTION ( 'NONE',  ( -3.885780586188016830E-16, -4.437342591868156373E-31, 1.000000000000000000 ) ) ;
#3829 = FACE_OUTER_BOUND ( 'NONE', #16269, .T. ) ;
#3830 = CARTESIAN_POINT ( 'NONE',  ( 4.175813232069142344, -2.061359961916371830, -3.570380186727398986 ) ) ;
#3831 = CIRCLE ( 'NONE', #5365, 0.4999999999999987232 ) ;
#3832 = CARTESIAN_POINT ( 'NONE',  ( 2.081668171172168513E-14, 10.00000000000000533, 0.000000000000000000 ) ) ;
#3833 = CARTESIAN_POINT ( 'NONE',  ( 12.84999999999997300, -1.999999999999998224, 0.000000000000000000 ) ) ;
#3834 = DIRECTION ( 'NONE',  ( 1.000000000000000000, -2.312964634635739999E-16, 1.302601544865244959E-30 ) ) ;
#3835 = PLANE ( 'NONE',  #17895 ) ;
#3836 = CARTESIAN_POINT ( 'NONE',  ( 6.495190528383244732, 4.999999999999948486, -3.750000000000000000 ) ) ;
#3837 = CARTESIAN_POINT ( 'NONE',  ( 37.22062532321636752, 10.88440674090235305, -10.54332536350028882 ) ) ;
#3838 = EDGE_CURVE ( 'NONE', #1775, #19103, #22548, .T. ) ;
#3839 = VECTOR ( 'NONE', #11903, 1000.000000000000000 ) ;
#3840 = CARTESIAN_POINT ( 'NONE',  ( 7.764145988665074327, -1.774864566462285520, 8.011880279048840592 ) ) ;
#3841 = CYLINDRICAL_SURFACE ( 'NONE', #2906, 0.5000000000000004441 ) ;
#3842 = AXIS2_PLACEMENT_3D ( 'NONE', #4437, #2804, #934 ) ;
#3843 = DIRECTION ( 'NONE',  ( -1.000000000000000000, -1.910522504832140594E-31, 5.551115123125818447E-17 ) ) ;
#3844 = CIRCLE ( 'NONE', #22257, 7.000000000000075495 ) ;
#3845 = CIRCLE ( 'NONE', #19262, 0.5000000000000038858 ) ;
#3846 = CARTESIAN_POINT ( 'NONE',  ( -42.54314575050796776, 3.999999999999996447, -8.000000000000035527 ) ) ;
#3847 = ORIENTED_EDGE ( 'NONE', *, *, #3053, .F. ) ;
#3848 = AXIS2_PLACEMENT_3D ( 'NONE', #9661, #4126, #9321 ) ;
#3849 = EDGE_LOOP ( 'NONE', ( #17324, #22882, #12393 ) ) ;
#3850 = CARTESIAN_POINT ( 'NONE',  ( -89.70000000000054285, -6.245004513516505540E-14, 1.000000000000000888 ) ) ;
#3851 = CARTESIAN_POINT ( 'NONE',  ( 110.6590008199704869, -13.16192875215410574, -6.000000000000047073 ) ) ;
#3852 = ORIENTED_EDGE ( 'NONE', *, *, #13872, .T. ) ;
#3853 = CIRCLE ( 'NONE', #5001, 0.5000000000000038858 ) ;
#3854 = DIRECTION ( 'NONE',  ( -2.013525853228507892E-32, -6.902532920683810383E-31, 1.000000000000000000 ) ) ;
#3855 = AXIS2_PLACEMENT_3D ( 'NONE', #6308, #7834, #6542 ) ;
#3856 = VECTOR ( 'NONE', #16275, 1000.000000000000000 ) ;
#3857 = DIRECTION ( 'NONE',  ( 0.5000000000000000000, 0.000000000000000000, -0.8660254037844385966 ) ) ;
#3858 = CARTESIAN_POINT ( 'NONE',  ( 4.158806965674322065, -1.986429158307121412, -3.559403772175879332 ) ) ;
#3859 = CARTESIAN_POINT ( 'NONE',  ( 12.84999999999997300, -14.00000000000011369, -5.749999999999921840 ) ) ;
#3860 = CARTESIAN_POINT ( 'NONE',  ( 57.15235153779110533, -1.074585193523325266, 6.500000000000117240 ) ) ;
#3861 = ORIENTED_EDGE ( 'NONE', *, *, #9614, .T. ) ;
#3862 = FACE_OUTER_BOUND ( 'NONE', #7428, .T. ) ;
#3863 = DIRECTION ( 'NONE',  ( -1.000000000000000000, 0.000000000000000000, 0.000000000000000000 ) ) ;
#3864 = CARTESIAN_POINT ( 'NONE',  ( 22.50000000000003908, 4.500000000000031974, -1.499999999999997780 ) ) ;
#3865 = CARTESIAN_POINT ( 'NONE',  ( 7.000000000000020428, -13.02884243125069652, 9.522727272727321335 ) ) ;
#3866 = EDGE_CURVE ( 'NONE', #9788, #4065, #12350, .T. ) ;
#3867 = CARTESIAN_POINT ( 'NONE',  ( 7.479729963978305918, -13.19653517305387780, 9.265052153035679083 ) ) ;
#3868 = CARTESIAN_POINT ( 'NONE',  ( 27.59619407800441948, 27.59619407671642222, -26.50000000000000000 ) ) ;
#3869 = DIRECTION ( 'NONE',  ( 1.000000000000000000, -4.190823558986610327E-31, 1.733449886265890494E-32 ) ) ;
#3870 = CARTESIAN_POINT ( 'NONE',  ( -6.938893903907228378E-14, 4.999999999999976907, -4.163336342344337027E-14 ) ) ;
#3871 = CARTESIAN_POINT ( 'NONE',  ( -1.318389841742373392E-16, -14.99999999999997335, -4.750000000000026645 ) ) ;
#3872 = VECTOR ( 'NONE', #2928, 1000.000000000000114 ) ;
#3873 = FACE_OUTER_BOUND ( 'NONE', #10394, .T. ) ;
#3874 = VECTOR ( 'NONE', #16784, 1000.000000000000000 ) ;
#3875 = CIRCLE ( 'NONE', #22689, 0.5000000000000038858 ) ;
#3876 = AXIS2_PLACEMENT_3D ( 'NONE', #873, #8043, #22397 ) ;
#3877 = AXIS2_PLACEMENT_3D ( 'NONE', #14829, #18472, #9539 ) ;
#3878 = STYLED_ITEM ( 'NONE', ( #724 ), #13118 ) ;
#3879 = APPLICATION_PROTOCOL_DEFINITION ( 'draft international standard', 'automotive_design', 1998, #10732 ) ;
#3880 = ORIENTED_EDGE ( 'NONE', *, *, #16542, .F. ) ;
#3881 = EDGE_CURVE ( 'NONE', #7229, #16003, #475, .T. ) ;
#3882 = ORIENTED_EDGE ( 'NONE', *, *, #22322, .T. ) ;
#3884 = ORIENTED_EDGE ( 'NONE', *, *, #16127, .T. ) ;
#3883 = ORIENTED_EDGE ( 'NONE', *, *, #3766, .F. ) ;
#3885 = DIRECTION ( 'NONE',  ( -3.885780586188016830E-16, -4.437342591868156373E-31, 1.000000000000000000 ) ) ;
#3886 = LINE ( 'NONE', #18473, #22378 ) ;
#3887 = EDGE_CURVE ( 'NONE', #10913, #15916, #10301, .T. ) ;
#3888 = VECTOR ( 'NONE', #3729, 1000.000000000000000 ) ;
#3889 = VECTOR ( 'NONE', #16964, 1000.000000000000000 ) ;
#3890 = DIRECTION ( 'NONE',  ( -0.7071067811865507924, -0.7071067811865444641, 7.226392596171890537E-15 ) ) ;
#3891 = TOROIDAL_SURFACE ( 'NONE', #8033, 6.700000000000001066, 0.5000000000000000000 ) ;
#3892 = CARTESIAN_POINT ( 'NONE',  ( 30.00000000029184832, -0.5000000009961480529, -8.549999999999997158 ) ) ;
#3893 = VECTOR ( 'NONE', #19141, 1000.000000000000000 ) ;
#3894 = CARTESIAN_POINT ( 'NONE',  ( -56.87767137932630845, -0.5000000000000281997, 8.833333333333401427 ) ) ;
#3895 = EDGE_CURVE ( 'NONE', #547, #19657, #1108, .T. ) ;
#3896 = DIRECTION ( 'NONE',  ( 0.000000000000000000, 1.000000000000000000, 0.000000000000000000 ) ) ;
#3897 = DIRECTION ( 'NONE',  ( -3.070652698126927723E-17, -1.000000000000000000, 4.167305704548413124E-17 ) ) ;
#3898 = FACE_OUTER_BOUND ( 'NONE', #11810, .T. ) ;
#3899 = DIRECTION ( 'NONE',  ( 0.000000000000000000, 0.000000000000000000, 1.000000000000000000 ) ) ;
#3900 = LINE ( 'NONE', #20498, #4673 ) ;
#3901 = CARTESIAN_POINT ( 'NONE',  ( 4.050536630291682982, -2.401306687817042818, 2.976670123173756899 ) ) ;
#3902 = ADVANCED_FACE ( 'NONE', ( #1024, #15701, #20903 ), #6433, .F. ) ;
#3903 = LINE ( 'NONE', #7559, #18323 ) ;
#3904 = ADVANCED_FACE ( 'NONE', ( #11709 ), #2782, .T. ) ;
#3905 = DIRECTION ( 'NONE',  ( 0.000000000000000000, 0.000000000000000000, -1.000000000000000000 ) ) ;
#3906 = CARTESIAN_POINT ( 'NONE',  ( 7.029812747553613406, -0.6228290751908035494, 8.933015330925462294 ) ) ;
#3907 = ORIENTED_EDGE ( 'NONE', *, *, #10827, .T. ) ;
#3908 = AXIS2_PLACEMENT_3D ( 'NONE', #7894, #11418, #16579 ) ;
#3909 = AXIS2_PLACEMENT_3D ( 'NONE', #22133, #4125, #18483 ) ;
#3911 = ORIENTED_EDGE ( 'NONE', *, *, #14153, .F. ) ;
#3910 = ORIENTED_EDGE ( 'NONE', *, *, #13856, .F. ) ;
#3912 = CIRCLE ( 'NONE', #7687, 2.100000000000011635 ) ;
#3913 = VERTEX_POINT ( 'NONE', #21017 ) ;
#3914 = VERTEX_POINT ( 'NONE', #4881 ) ;
#3916 = ORIENTED_EDGE ( 'NONE', *, *, #21643, .F. ) ;
#3915 = VERTEX_POINT ( 'NONE', #12049 ) ;
#3917 = ORIENTED_EDGE ( 'NONE', *, *, #14247, .F. ) ;
#3918 = DIRECTION ( 'NONE',  ( 2.172745813409349776E-17, -1.000000000000000000, 1.309377075419428048E-16 ) ) ;
#3919 = EDGE_CURVE ( 'NONE', #19599, #16893, #18377, .T. ) ;
#3920 = ORIENTED_EDGE ( 'NONE', *, *, #2017, .F. ) ;
#3921 = ORIENTED_EDGE ( 'NONE', *, *, #23210, .F. ) ;
#3922 = EDGE_CURVE ( 'NONE', #16601, #15739, #8891, .T. ) ;
#3923 = CARTESIAN_POINT ( 'NONE',  ( 4.000000000000003553, 1.935983797701078757, -0.2494693066162351203 ) ) ;
#3924 = EDGE_CURVE ( 'NONE', #16351, #1669, #7845, .T. ) ;
#3925 = DIRECTION ( 'NONE',  ( 1.000000000000000000, -1.550910762415513985E-16, -3.012982189080959477E-32 ) ) ;
#3926 = LINE ( 'NONE', #3808, #9397 ) ;
#3927 = DIRECTION ( 'NONE',  ( 5.551115123561405253E-17, 1.000000000000000000, -5.963788443470795439E-28 ) ) ;
#3928 = AXIS2_PLACEMENT_3D ( 'NONE', #1194, #4936, #10013 ) ;
#3929 = CARTESIAN_POINT ( 'NONE',  ( 2.775557561562891351E-14, 7.999999999999983125, -0.4999999999999865663 ) ) ;
#3930 = CIRCLE ( 'NONE', #9209, 4.000000000000023093 ) ;
#3931 = CARTESIAN_POINT ( 'NONE',  ( 2.918498775983380256E-10, 2.999999999003851503, -19.00000000000000355 ) ) ;
#3932 = CARTESIAN_POINT ( 'NONE',  ( 4.175813232069149450, -4.122719923832729449, 0.000000000000000000 ) ) ;
#3933 = EDGE_CURVE ( 'NONE', #9334, #16286, #1462, .T. ) ;
#3934 = CARTESIAN_POINT ( 'NONE',  ( 4.113620667976089607, 1.749999999999973799, 2.375000000000000444 ) ) ;
#3935 = CARTESIAN_POINT ( 'NONE',  ( -45.56568542494964191, 2.108831175456925333, -8.000000000000062172 ) ) ;
#3936 = EDGE_CURVE ( 'NONE', #1743, #10125, #8235, .T. ) ;
#3937 = CARTESIAN_POINT ( 'NONE',  ( 37.54332536350037230, 10.88440674090231752, -2.779374676783941567 ) ) ;
#3938 = EDGE_CURVE ( 'NONE', #23066, #9452, #17236, .T. ) ;
#3939 = ORIENTED_EDGE ( 'NONE', *, *, #6350, .T. ) ;
#3940 = UNCERTAINTY_MEASURE_WITH_UNIT (LENGTH_MEASURE( 1.000000000000000082E-05 ), #22291, 'distance_accuracy_value', 'NONE');
#3941 = DIRECTION ( 'NONE',  ( -0.000000000000000000, -0.000000000000000000, 1.000000000000000000 ) ) ;
#3943 = VERTEX_POINT ( 'NONE', #1823 ) ;
#3942 = ORIENTED_EDGE ( 'NONE', *, *, #14570, .T. ) ;
#3944 = ORIENTED_EDGE ( 'NONE', *, *, #22340, .F. ) ;
#3945 = VECTOR ( 'NONE', #14091, 1000.000000000000000 ) ;
#3946 = ORIENTED_EDGE ( 'NONE', *, *, #20317, .F. ) ;
#3947 = VECTOR ( 'NONE', #7543, 1000.000000000000000 ) ;
#3948 = ORIENTED_EDGE ( 'NONE', *, *, #15817, .F. ) ;
#3949 = ORIENTED_EDGE ( 'NONE', *, *, #9809, .T. ) ;
#3950 = DIRECTION ( 'NONE',  ( 2.775557561562886113E-17, -2.775557561562883955E-16, 1.000000000000000000 ) ) ;
#3951 = DIRECTION ( 'NONE',  ( -1.331202777560457422E-30, -1.000000000000000000, 7.395570986446985676E-31 ) ) ;
#3952 = CYLINDRICAL_SURFACE ( 'NONE', #6841, 0.5000000000000022204 ) ;
#3953 = DIRECTION ( 'NONE',  ( -1.000000000000000000, 1.550910762415526064E-16, 0.000000000000000000 ) ) ;
#3954 = DIRECTION ( 'NONE',  ( -0.7071067811865457964, -0.7071067811865492381, 0.000000000000000000 ) ) ;
#3955 = CARTESIAN_POINT ( 'NONE',  ( 12.84999999999997300, -1.999999999999998224, 0.000000000000000000 ) ) ;
#3956 = ADVANCED_FACE ( 'NONE', ( #12522 ), #20261, .T. ) ;
#3957 = LINE ( 'NONE', #21847, #11492 ) ;
#3958 = CARTESIAN_POINT ( 'NONE',  ( -7.761744141695535504, -2.064358047808336316, 6.973942750959534642 ) ) ;
#3959 = CARTESIAN_POINT ( 'NONE',  ( -0.7206956945560391015, 4.999999999999988454, -7.500000000000003553 ) ) ;
#3960 = AXIS2_PLACEMENT_3D ( 'NONE', #17877, #10574, #14232 ) ;
#3961 = DIRECTION ( 'NONE',  ( 4.615739097524196635E-16, -1.000000000000000000, -2.220446049250317025E-16 ) ) ;
#3962 = APPLICATION_CONTEXT ( 'automotive_design' ) ;
#3963 = DIRECTION ( 'NONE',  ( 1.577021341797097314E-16, 1.000000000000000000, -1.734723475976807094E-15 ) ) ;
#3964 = EDGE_CURVE ( 'NONE', #11851, #6388, #10519, .T. ) ;
#3965 = VECTOR ( 'NONE', #15778, 1000.000000000000000 ) ;
#3966 = DIRECTION ( 'NONE',  ( -5.551115123561405253E-17, -1.000000000000000000, -2.256980353643891447E-27 ) ) ;
#3967 = DIRECTION ( 'NONE',  ( -1.000000000000000000, -3.254448077276381206E-32, -1.066788928082016908E-26 ) ) ;
#3968 = B_SPLINE_CURVE_WITH_KNOTS ( 'NONE', 3,
 ( #3194, #8593, #22957, #21875, #19883 ),
 .UNSPECIFIED., .F., .F.,
 ( 4, 1, 4 ),
 ( 0.000000000000000000, 0.002020725942163685736, 0.004041451884327371472 ),
 .UNSPECIFIED. ) ;
#3969 = CIRCLE ( 'NONE', #22758, 0.4999999999999995559 ) ;
#3970 = VERTEX_POINT ( 'NONE', #19477 ) ;
#3971 = CARTESIAN_POINT ( 'NONE',  ( -4.239424077913607647, 37.80035007138369707, -28.99269273888553400 ) ) ;
#3972 = CARTESIAN_POINT ( 'NONE',  ( 24.75000000000001066, 2.000000000000099032, -16.99999999999999289 ) ) ;
#3973 = ORIENTED_EDGE ( 'NONE', *, *, #15996, .F. ) ;
#3974 = DIRECTION ( 'NONE',  ( -1.066788928082016908E-26, 6.656013887802287108E-31, 1.000000000000000000 ) ) ;
#3975 = DIRECTION ( 'NONE',  ( 2.563050070131097656E-17, -0.7071067811865543451, 0.7071067811865406894 ) ) ;
#3976 = CARTESIAN_POINT ( 'NONE',  ( 4.086376042167614742, -4.082715877136890548, 0.07147133206913598713 ) ) ;
#3977 = LINE ( 'NONE', #9403, #12829 ) ;
#3978 = CYLINDRICAL_SURFACE ( 'NONE', #19896, 0.4999999999999995559 ) ;
#3979 = CARTESIAN_POINT ( 'NONE',  ( -12.85000000000001386, -13.50000000000007105, 5.551115123125782702E-14 ) ) ;
#3980 = CARTESIAN_POINT ( 'NONE',  ( 108.2426266706970353, -11.02760560296359138, -6.000000000000019540 ) ) ;
#3981 = CYLINDRICAL_SURFACE ( 'NONE', #8672, 0.5000000000000004441 ) ;
#3982 = CARTESIAN_POINT ( 'NONE',  ( 7.271441198316241916, -13.72907106061213511, 8.039702399269780031 ) ) ;
#3983 = VECTOR ( 'NONE', #17623, 1000.000000000000000 ) ;
#3984 = DIRECTION ( 'NONE',  ( 2.013525853228507892E-32, 6.902532920683810383E-31, -1.000000000000000000 ) ) ;
#3985 = DIRECTION ( 'NONE',  ( -1.000000000000000000, 3.469446951953575061E-14, 0.000000000000000000 ) ) ;
#3986 = DIRECTION ( 'NONE',  ( -1.000000000000000000, -1.479114197289387852E-30, 2.013525853228518840E-32 ) ) ;
#3987 = FACE_OUTER_BOUND ( 'NONE', #12599, .T. ) ;
#3988 = FILL_AREA_STYLE ('',( #711 ) ) ;
#3989 = EDGE_CURVE ( 'NONE', #138, #10463, #16161, .T. ) ;
#3990 = CARTESIAN_POINT ( 'NONE',  ( 4.165266963751725449, 2.049631966911992453, -3.550066703508908184 ) ) ;
#3991 = CIRCLE ( 'NONE', #11869, 0.4999999999999992228 ) ;
#3992 = AXIS2_PLACEMENT_3D ( 'NONE', #13338, #20637, #2505 ) ;
#3993 = APPLICATION_PROTOCOL_DEFINITION ( 'draft international standard', 'automotive_design', 1998, #2765 ) ;
#3994 = EDGE_LOOP ( 'NONE', ( #19954, #15374, #12009 ) ) ;
#3995 = CIRCLE ( 'NONE', #4359, 0.5000000000000038858 ) ;
#3996 = EDGE_CURVE ( 'NONE', #14430, #3527, #20144, .T. ) ;
#3998 = ORIENTED_EDGE ( 'NONE', *, *, #10158, .T. ) ;
#3997 = EDGE_LOOP ( 'NONE', ( #8633, #17846, #6661, #1968 ) ) ;
#3999 = PRESENTATION_LAYER_ASSIGNMENT (  '', '', ( #15264 ) ) ;
#4000 = CARTESIAN_POINT ( 'NONE',  ( 36.00000000029184832, 16.99999999900385461, -26.50000000000000000 ) ) ;
#4001 = CARTESIAN_POINT ( 'NONE',  ( 7.000000000000006217, -0.9711575687493152476, 9.522727272727294690 ) ) ;
#4002 = CARTESIAN_POINT ( 'NONE',  ( 7.710998176012808791, -11.54387914083316424, 8.114728912742409150 ) ) ;
#4003 = ORIENTED_EDGE ( 'NONE', *, *, #11324, .F. ) ;
#4004 = CARTESIAN_POINT ( 'NONE',  ( 4.082498951862918446, 4.041451884327377009, -2.081668171172168513E-14 ) ) ;
#4005 = LINE ( 'NONE', #16472, #20690 ) ;
#4006 = DIRECTION ( 'NONE',  ( -0.5000000000000055511, -0.8660254037844354880, 0.000000000000000000 ) ) ;
#4007 = CARTESIAN_POINT ( 'NONE',  ( -45.56568542494954244, -2.700000000000091216, -7.500000000000062172 ) ) ;
#4008 = DIRECTION ( 'NONE',  ( 0.000000000000000000, 0.000000000000000000, -1.000000000000000000 ) ) ;
#4009 = VECTOR ( 'NONE', #17544, 1000.000000000000000 ) ;
#4010 = CARTESIAN_POINT ( 'NONE',  ( 8.697224362267983011, -1.999999999999984457, 6.249999999999992006 ) ) ;
#4011 = CARTESIAN_POINT ( 'NONE',  ( -43.10883117545713361, -4.565685424949276872, 8.000000000000035527 ) ) ;
#4012 = CARTESIAN_POINT ( 'NONE',  ( 4.203833317240822431, 1.627343821129635382, -3.597273115243896591 ) ) ;
#4013 =( NAMED_UNIT ( * ) SI_UNIT ( $, .STERADIAN. ) SOLID_ANGLE_UNIT ( ) );
#4014 = FACE_OUTER_BOUND ( 'NONE', #5435, .T. ) ;
#4015 = AXIS2_PLACEMENT_3D ( 'NONE', #18838, #8023, #13436 ) ;
#4016 = CARTESIAN_POINT ( 'NONE',  ( 2.000000000000015543, -3.464101615137746837, -5.600000000000000533 ) ) ;
#4017 = CARTESIAN_POINT ( 'NONE',  ( -50.65685424949281668, 1.387778780781445676E-14, 7.500000000000034639 ) ) ;
#4018 = CARTESIAN_POINT ( 'NONE',  ( 42.50000000000023448, 10.49999999999999822, 2.500000000000002220 ) ) ;
#4019 = CARTESIAN_POINT ( 'NONE',  ( 7.613388670473284492, -0.8883455870200749338, 8.423574099071707622 ) ) ;
#4020 = ORIENTED_EDGE ( 'NONE', *, *, #12395, .T. ) ;
#4021 = EDGE_CURVE ( 'NONE', #13762, #13703, #16544, .T. ) ;
#4022 = AXIS2_PLACEMENT_3D ( 'NONE', #4910, #11626, #19158 ) ;
#4024 = ORIENTED_EDGE ( 'NONE', *, *, #13838, .T. ) ;
#4023 = VERTEX_POINT ( 'NONE', #16046 ) ;
#4025 = EDGE_CURVE ( 'NONE', #9067, #5868, #19854, .T. ) ;
#4026 = EDGE_LOOP ( 'NONE', ( #10568, #22388, #18994, #18617 ) ) ;
#4027 = ORIENTED_EDGE ( 'NONE', *, *, #15274, .T. ) ;
#4029 = VERTEX_POINT ( 'NONE', #14302 ) ;
#4028 = ORIENTED_EDGE ( 'NONE', *, *, #13447, .T. ) ;
#4030 = AXIS2_PLACEMENT_3D ( 'NONE', #2106, #1871, #9055 ) ;
#4031 = ORIENTED_EDGE ( 'NONE', *, *, #1360, .F. ) ;
#4032 = FACE_OUTER_BOUND ( 'NONE', #10632, .T. ) ;
#4033 = ORIENTED_EDGE ( 'NONE', *, *, #19604, .F. ) ;
#4034 = ORIENTED_EDGE ( 'NONE', *, *, #6957, .F. ) ;
#4035 = LINE ( 'NONE', #14406, #173 ) ;
#4036 = EDGE_CURVE ( 'NONE', #21802, #18939, #16057, .T. ) ;
#4037 = FILL_AREA_STYLE ('',( #17938 ) ) ;
#4038 = CIRCLE ( 'NONE', #13062, 2.500000000000003553 ) ;
#4039 = CARTESIAN_POINT ( 'NONE',  ( -64.00000000000045475, -0.5000000000000628386, -2.000000000000001776 ) ) ;
#4040 = EDGE_CURVE ( 'NONE', #16175, #15826, #19720, .T. ) ;
#4041 = DIRECTION ( 'NONE',  ( 0.000000000000000000, 0.000000000000000000, 1.000000000000000000 ) ) ;
#4042 = AXIS2_PLACEMENT_3D ( 'NONE', #13320, #5809, #6028 ) ;
#4043 = PLANE ( 'NONE',  #21161 ) ;
#4044 = FACE_OUTER_BOUND ( 'NONE', #1497, .T. ) ;
#4045 = PLANE ( 'NONE',  #1679 ) ;
#4046 = VECTOR ( 'NONE', #11331, 1000.000000000000114 ) ;
#4047 = DIRECTION ( 'NONE',  ( 0.000000000000000000, 0.000000000000000000, -1.000000000000000000 ) ) ;
#4048 = AXIS2_PLACEMENT_3D ( 'NONE', #9153, #21517, #23046 ) ;
#4049 = CARTESIAN_POINT ( 'NONE',  ( 10.50000000000000888, -0.5000000000000004441, 9.250000000000008882 ) ) ;
#4050 = CIRCLE ( 'NONE', #1804, 4.999999999999999112 ) ;
#4051 = ORIENTED_EDGE ( 'NONE', *, *, #19935, .F. ) ;
#4052 = EDGE_CURVE ( 'NONE', #3456, #10401, #10761, .T. ) ;
#4053 = ADVANCED_FACE ( 'NONE', ( #9009 ), #14416, .T. ) ;
#4054 =( NAMED_UNIT ( * ) PLANE_ANGLE_UNIT ( ) SI_UNIT ( $, .RADIAN. ) );
#4055 = PLANE ( 'NONE',  #11234 ) ;
#4057 = ORIENTED_EDGE ( 'NONE', *, *, #5652, .F. ) ;
#4056 = ORIENTED_EDGE ( 'NONE', *, *, #19456, .F. ) ;
#4058 = VECTOR ( 'NONE', #20823, 1000.000000000000000 ) ;
#4059 = ADVANCED_FACE ( 'NONE', ( #19359 ), #4799, .T. ) ;
#4060 = ORIENTED_EDGE ( 'NONE', *, *, #9572, .F. ) ;
#4061 = VECTOR ( 'NONE', #19050, 1000.000000000000000 ) ;
#4062 = VERTEX_POINT ( 'NONE', #12763 ) ;
#4063 = CIRCLE ( 'NONE', #10083, 0.5000000000000000000 ) ;
#4064 = ORIENTED_EDGE ( 'NONE', *, *, #3386, .T. ) ;
#4065 = VERTEX_POINT ( 'NONE', #16392 ) ;
#4066 = CARTESIAN_POINT ( 'NONE',  ( 30.00000000029184832, 2.999999999003851503, 0.000000000000000000 ) ) ;
#4067 = EDGE_CURVE ( 'NONE', #3237, #9334, #11925, .T. ) ;
#4068 = DIRECTION ( 'NONE',  ( -0.4999999999999998335, -4.767331059895059913E-16, -0.8660254037844387076 ) ) ;
#4069 = ADVANCED_FACE ( 'NONE', ( #20407 ), #21351, .T. ) ;
#4070 = CARTESIAN_POINT ( 'NONE',  ( 36.00000000029184832, 49.99999999900385461, -28.99999999999999645 ) ) ;
#4071 = DIRECTION ( 'NONE',  ( 1.000000000000000000, -1.389842848855773367E-62, 2.013525853228507892E-32 ) ) ;
#4072 = CARTESIAN_POINT ( 'NONE',  ( 25.15499999999999403, 0.000000000000000000, -6.938893903907228378E-15 ) ) ;
#4073 = DIRECTION ( 'NONE',  ( 0.000000000000000000, 0.000000000000000000, -1.000000000000000000 ) ) ;
#4074 = CARTESIAN_POINT ( 'NONE',  ( -7.734741761309930297, -11.93000978614838559, 7.004299047562723146 ) ) ;
#4075 = CARTESIAN_POINT ( 'NONE',  ( -7.479729963973698936, -13.19653517305877166, 9.265052153039251337 ) ) ;
#4076 = VECTOR ( 'NONE', #223, 1000.000000000000000 ) ;
#4077 = LINE ( 'NONE', #11254, #3711 ) ;
#4078 = CIRCLE ( 'NONE', #2962, 0.4999999999999995559 ) ;
#4079 = CARTESIAN_POINT ( 'NONE',  ( 8.832214555408109291, -1.499999999999984457, 6.752214322824766413 ) ) ;
#4080 = CYLINDRICAL_SURFACE ( 'NONE', #3609, 0.4999999999999995559 ) ;
#4081 = EDGE_CURVE ( 'NONE', #7132, #10391, #8325, .T. ) ;
#4082 = EDGE_CURVE ( 'NONE', #10053, #20034, #5945, .T. ) ;
#4083 = CARTESIAN_POINT ( 'NONE',  ( 3.000000000291852764, 42.99999999900385461, -26.00000000000000000 ) ) ;
#4084 = FACE_OUTER_BOUND ( 'NONE', #4644, .T. ) ;
#4085 = ORIENTED_EDGE ( 'NONE', *, *, #10217, .F. ) ;
#4086 = ADVANCED_FACE ( 'NONE', ( #13224 ), #14204, .F. ) ;
#4087 = DIRECTION ( 'NONE',  ( 2.168404344970994323E-16, -1.000000000000000000, 1.577721810442023611E-30 ) ) ;
#4088 = AXIS2_PLACEMENT_3D ( 'NONE', #17240, #18788, #921 ) ;
#4089 = CYLINDRICAL_SURFACE ( 'NONE', #8335, 0.5000000000000004441 ) ;
#4090 = VERTEX_POINT ( 'NONE', #2286 ) ;
#4091 = B_SPLINE_CURVE_WITH_KNOTS ( 'NONE', 3,
 ( #15178, #22371, #6253, #5032, #2836, #20606 ),
 .UNSPECIFIED., .F., .F.,
 ( 4, 2, 4 ),
 ( 0.000000000000000000, 0.002086519881787258883, 0.004173039763574517766 ),
 .UNSPECIFIED. ) ;
#4092 = CARTESIAN_POINT ( 'NONE',  ( -6.000000000000074607, -8.000000000000003553, -7.500000000000034639 ) ) ;
#4093 = FACE_OUTER_BOUND ( 'NONE', #17455, .T. ) ;
#4094 = DIRECTION ( 'NONE',  ( 1.000000000000000000, 0.000000000000000000, 0.000000000000000000 ) ) ;
#4095 = CARTESIAN_POINT ( 'NONE',  ( -12.84999999999999964, -0.5000000000000004441, -5.749999999999963585 ) ) ;
#4096 = FACE_OUTER_BOUND ( 'NONE', #13381, .T. ) ;
#4097 = DIRECTION ( 'NONE',  ( 0.000000000000000000, 0.000000000000000000, 1.000000000000000000 ) ) ;
#4098 = CARTESIAN_POINT ( 'NONE',  ( 3.674234614174737068, 0.7500000000000492939, -3.000000000000002665 ) ) ;
#4099 = DIRECTION ( 'NONE',  ( -1.000000000000000000, 4.440892098500650814E-16, 7.860214984771115307E-18 ) ) ;
#4100 =( GEOMETRIC_REPRESENTATION_CONTEXT ( 3 ) GLOBAL_UNCERTAINTY_ASSIGNED_CONTEXT ( ( #6296 ) ) GLOBAL_UNIT_ASSIGNED_CONTEXT ( ( #21237, #19567, #20036 ) ) REPRESENTATION_CONTEXT ( 'NONE', 'WORKASPACE' ) );
#4101 = DIRECTION ( 'NONE',  ( 0.000000000000000000, 1.000000000000000000, 0.000000000000000000 ) ) ;
#4102 = DIRECTION ( 'NONE',  ( 0.000000000000000000, 0.000000000000000000, -1.000000000000000000 ) ) ;
#4103 = LINE ( 'NONE', #20114, #11373 ) ;
#4104 = DIRECTION ( 'NONE',  ( -3.241725282392603095E-30, -1.000000000000000000, 2.218671295934100958E-31 ) ) ;
#4105 = SURFACE_STYLE_FILL_AREA ( #11053 ) ;
#4106 = CARTESIAN_POINT ( 'NONE',  ( 0.000000000000000000, 0.000000000000000000, 0.000000000000000000 ) ) ;
#4107 = AXIS2_PLACEMENT_3D ( 'NONE', #6544, #4531, #17339 ) ;
#4108 = EDGE_LOOP ( 'NONE', ( #3739, #20862, #14959, #13007 ) ) ;
#4109 = ADVANCED_FACE ( 'NONE', ( #20176, #4272 ), #2404, .T. ) ;
#4110 = COLOUR_RGB ( '', 0.31764706, 0.68627451, 0.89019608) ;
#4112 = ORIENTED_EDGE ( 'NONE', *, *, #21745, .F. ) ;
#4111 = VERTEX_POINT ( 'NONE', #21947 ) ;
#4113 = DIRECTION ( 'NONE',  ( -1.000000000000000000, -4.440892098500626162E-16, 5.551115123125782702E-16 ) ) ;
#4114 = EDGE_CURVE ( 'NONE', #6361, #19223, #536, .T. ) ;
#4115 = DIRECTION ( 'NONE',  ( 8.438582421954109416E-32, 0.000000000000000000, 1.000000000000000000 ) ) ;
#4116 = CYLINDRICAL_SURFACE ( 'NONE', #9905, 0.5000000000000000000 ) ;
#4117 = EDGE_LOOP ( 'NONE', ( #7484, #18129 ) ) ;
#4118 = DIRECTION ( 'NONE',  ( -2.013525853228507892E-32, -6.902532920683810383E-31, 1.000000000000000000 ) ) ;
#4119 = CARTESIAN_POINT ( 'NONE',  ( 2.499999999999988454, 4.500000000000059508, -3.469446951953614189E-14 ) ) ;
#4120 = CARTESIAN_POINT ( 'NONE',  ( -3.122502256758252770E-14, 59.74999999999991473, 2.081668171172168513E-14 ) ) ;
#4121 = CARTESIAN_POINT ( 'NONE',  ( -55.25320565519152893, 2.700000000000104983, 8.000000000000035527 ) ) ;
#4122 = CARTESIAN_POINT ( 'NONE',  ( 0.000000000000000000, 1.750000000000001554, 0.000000000000000000 ) ) ;
#4123 = CYLINDRICAL_SURFACE ( 'NONE', #16208, 4.749999999999986677 ) ;
#4124 = CONICAL_SURFACE ( 'NONE', #13894, 4.000000000000000000, 1.047197551196595855 ) ;
#4125 = DIRECTION ( 'NONE',  ( -1.000000000000000000, -3.254448077276381206E-32, -1.066788928082016908E-26 ) ) ;
#4126 = DIRECTION ( 'NONE',  ( 7.860214984770699307E-18, -1.409037165336591006E-16, -1.000000000000000000 ) ) ;
#4127 = PLANE ( 'NONE',  #18459 ) ;
#4128 = CARTESIAN_POINT ( 'NONE',  ( 55.36587326203800075, 4.009651402420072230, -6.499999999999977796 ) ) ;
#4129 = CARTESIAN_POINT ( 'NONE',  ( 6.999999999999978684, -2.818969682667037624, 8.693499985977959810 ) ) ;
#4130 = CARTESIAN_POINT ( 'NONE',  ( -5.623500955413251567, 35.99999999900384751, -19.26867706693546367 ) ) ;
#4131 = DIRECTION ( 'NONE',  ( -0.7071067811865535679, -0.7071067811865414665, 0.000000000000000000 ) ) ;
#4132 = VERTEX_POINT ( 'NONE', #18634 ) ;
#4133 = ADVANCED_FACE ( 'NONE', ( #7704 ), #22055, .F. ) ;
#4134 = APPLICATION_PROTOCOL_DEFINITION ( 'draft international standard', 'automotive_design', 1998, #11146 ) ;
#4136 = ORIENTED_EDGE ( 'NONE', *, *, #14675, .F. ) ;
#4135 = ORIENTED_EDGE ( 'NONE', *, *, #15331, .F. ) ;
#4137 = UNCERTAINTY_MEASURE_WITH_UNIT (LENGTH_MEASURE( 1.000000000000000082E-05 ), #21562, 'distance_accuracy_value', 'NONE');
#4138 = ORIENTED_EDGE ( 'NONE', *, *, #4784, .F. ) ;
#4139 = VERTEX_POINT ( 'NONE', #9466 ) ;
#4141 = EDGE_LOOP ( 'NONE', ( #8555, #21837, #8518, #10796 ) ) ;
#4140 = ORIENTED_EDGE ( 'NONE', *, *, #8474, .F. ) ;
#4142 = EDGE_LOOP ( 'NONE', ( #5785, #9358, #4305, #4518 ) ) ;
#4143 = CARTESIAN_POINT ( 'NONE',  ( 113.0166151911345906, -11.64708151429785765, 6.000000000000067502 ) ) ;
#4144 = VERTEX_POINT ( 'NONE', #16857 ) ;
#4145 = ORIENTED_EDGE ( 'NONE', *, *, #5242, .T. ) ;
#4146 =( LENGTH_UNIT ( ) NAMED_UNIT ( * ) SI_UNIT ( .MILLI., .METRE. ) );
#4147 = CARTESIAN_POINT ( 'NONE',  ( 0.1388410611046231868, -3.710337782248059657, -0.5735064479039724272 ) ) ;
#4148 = FACE_OUTER_BOUND ( 'NONE', #16917, .T. ) ;
#4149 = DIRECTION ( 'NONE',  ( 2.172745813409349776E-17, -1.000000000000000000, 1.309377075419428048E-16 ) ) ;
#4150 = B_SPLINE_CURVE_WITH_KNOTS ( 'NONE', 3,
 ( #8107, #15504, #8337, #8461 ),
 .UNSPECIFIED., .F., .F.,
 ( 4, 4 ),
 ( 0.002080789711329242460, 0.004173039763574508225 ),
 .UNSPECIFIED. ) ;
#4151 = CARTESIAN_POINT ( 'NONE',  ( -7.523705677352342747, -2.838350495272803364, 8.715168381933473540 ) ) ;
#4152 = CARTESIAN_POINT ( 'NONE',  ( 4.093692494532773729, -2.021783646005778312, -3.501831996793871582 ) ) ;
#4153 = DIRECTION ( 'NONE',  ( 0.000000000000000000, 1.000000000000000000, 0.000000000000000000 ) ) ;
#4154 = CARTESIAN_POINT ( 'NONE',  ( 119.5756419024615838, -7.000000000000062172, -6.000000000000019540 ) ) ;
#4155 = CYLINDRICAL_SURFACE ( 'NONE', #7231, 5.999999999999991118 ) ;
#4156 = ADVANCED_FACE ( 'NONE', ( #19947 ), #2514, .F. ) ;
#4157 = LINE ( 'NONE', #3935, #4046 ) ;
#4158 = CIRCLE ( 'NONE', #17303, 0.5000000000000022204 ) ;
#4159 = CARTESIAN_POINT ( 'NONE',  ( 12.49999999999995914, 2.775557561562891982E-14, -4.750000000000002665 ) ) ;
#4160 = ORIENTED_EDGE ( 'NONE', *, *, #2993, .F. ) ;
#4161 = PRODUCT_DEFINITION_CONTEXT ( 'detailed design', #1425, 'design' ) ;
#4162 = DIRECTION ( 'NONE',  ( 1.000000000000000000, 2.220446049250313081E-16, -3.656342123407104498E-48 ) ) ;
#4164 = VERTEX_POINT ( 'NONE', #21714 ) ;
#4163 = VERTEX_POINT ( 'NONE', #11229 ) ;
#4165 = VERTEX_POINT ( 'NONE', #298 ) ;
#4166 = ORIENTED_EDGE ( 'NONE', *, *, #16706, .F. ) ;
#4167 = EDGE_CURVE ( 'NONE', #7485, #21891, #4157, .T. ) ;
#4168 = ORIENTED_EDGE ( 'NONE', *, *, #18622, .T. ) ;
#4169 = VERTEX_POINT ( 'NONE', #5603 ) ;
#4170 = DIRECTION ( 'NONE',  ( 0.9878135252003127365, 2.193386639427060722E-16, -0.1556420233463029767 ) ) ;
#4171 = AXIS2_PLACEMENT_3D ( 'NONE', #10760, #13080, #14952 ) ;
#4172 = PLANE ( 'NONE',  #18509 ) ;
#4173 = ORIENTED_EDGE ( 'NONE', *, *, #1392, .F. ) ;
#4174 = CARTESIAN_POINT ( 'NONE',  ( 4.104070371397483541, -4.047367226856738220, 0.000000000000000000 ) ) ;
#4175 = EDGE_CURVE ( 'NONE', #12275, #9470, #5943, .T. ) ;
#4176 = CARTESIAN_POINT ( 'NONE',  ( -1.828356344711745018, -3.563200125723226197, -6.548411715222995921E-14 ) ) ;
#4177 = CARTESIAN_POINT ( 'NONE',  ( -3.999999999708153453, 13.99999999900385106, -22.50000000000000000 ) ) ;
#4178 = DIRECTION ( 'NONE',  ( 0.9706398123736300620, 1.281898970984135951E-30, 0.2405376366294562085 ) ) ;
#4179 = CARTESIAN_POINT ( 'NONE',  ( -7.638377885296727676, -12.06377841978599363, 8.340398698103474118 ) ) ;
#4180 = EDGE_CURVE ( 'NONE', #19813, #3717, #2932, .T. ) ;
#4181 = CARTESIAN_POINT ( 'NONE',  ( -7.742458795615090317, -13.26006887186487937, 8.061568688626005397 ) ) ;
#4182 = FACE_OUTER_BOUND ( 'NONE', #21170, .T. ) ;
#4183 = EDGE_CURVE ( 'NONE', #9648, #19280, #16507, .T. ) ;
#4184 = CARTESIAN_POINT ( 'NONE',  ( -50.65685424949263904, -7.200000000000071232, -7.500000000000034639 ) ) ;
#4186 = VECTOR ( 'NONE', #4295, 1000.000000000000000 ) ;
#4185 = DIRECTION ( 'NONE',  ( 5.551115123125796261E-17, -2.869019762633796499E-16, -1.000000000000000000 ) ) ;
#4187 = EDGE_CURVE ( 'NONE', #23027, #12123, #295, .T. ) ;
#4188 = ORIENTED_EDGE ( 'NONE', *, *, #7013, .F. ) ;
#4189 = ORIENTED_EDGE ( 'NONE', *, *, #5953, .F. ) ;
#4190 = ORIENTED_EDGE ( 'NONE', *, *, #2761, .F. ) ;
#4191 = CARTESIAN_POINT ( 'NONE',  ( -6.056833031243686882, 36.14537244600960264, -28.19628802432849213 ) ) ;
#4192 = CARTESIAN_POINT ( 'NONE',  ( -4.000000000000003553, -1.933795701539609446, -5.351162342337700828 ) ) ;
#4193 = ORIENTED_EDGE ( 'NONE', *, *, #11651, .T. ) ;
#4194 = AXIS2_PLACEMENT_3D ( 'NONE', #6625, #13802, #2986 ) ;
#4195 = DIRECTION ( 'NONE',  ( -1.733449886265890494E-32, 7.264582621685754939E-63, 1.000000000000000000 ) ) ;
#4196 = DIRECTION ( 'NONE',  ( 0.000000000000000000, 0.000000000000000000, 1.000000000000000000 ) ) ;
#4197 = ADVANCED_FACE ( 'NONE', ( #22753 ), #18327, .T. ) ;
#4198 = DIRECTION ( 'NONE',  ( 7.860214984771176937E-18, 1.409037165336591006E-16, 1.000000000000000000 ) ) ;
#4199 = EDGE_CURVE ( 'NONE', #2238, #19516, #11678, .T. ) ;
#4200 = EDGE_CURVE ( 'NONE', #11578, #13324, #7430, .T. ) ;
#4201 = DIRECTION ( 'NONE',  ( -4.019602852144215652E-47, -6.982962677686261977E-15, -1.000000000000000000 ) ) ;
#4202 = CARTESIAN_POINT ( 'NONE',  ( 73.50000000000116529, -13.52760560296348302, 2.550000000000047340 ) ) ;
#4203 = DIRECTION ( 'NONE',  ( -1.000000000000000000, 1.550910762415566494E-16, 1.495339968488870838E-47 ) ) ;
#4204 = AXIS2_PLACEMENT_3D ( 'NONE', #19254, #10319, #8794 ) ;
#4205 = CIRCLE ( 'NONE', #20761, 2.549999999999997158 ) ;
#4206 = CARTESIAN_POINT ( 'NONE',  ( 7.028413389564970970, -13.36994781876315486, 8.946655872546040555 ) ) ;
#4207 = DIRECTION ( 'NONE',  ( 0.000000000000000000, 0.000000000000000000, -1.000000000000000000 ) ) ;
#4208 = CARTESIAN_POINT ( 'NONE',  ( 0.000000000000000000, 0.000000000000000000, -5.000000000000000888 ) ) ;
#4209 = DIRECTION ( 'NONE',  ( 0.000000000000000000, 0.000000000000000000, -1.000000000000000000 ) ) ;
#4210 = CARTESIAN_POINT ( 'NONE',  ( -3.674234614174765046, 0.7500000000000630607, -2.999999999999995559 ) ) ;
#4211 = EDGE_CURVE ( 'NONE', #23028, #278, #1418, .T. ) ;
#4212 = SURFACE_SIDE_STYLE ('',( #4105 ) ) ;
#4213 = EDGE_CURVE ( 'NONE', #6944, #21173, #6407, .T. ) ;
#4214 = MECHANICAL_DESIGN_GEOMETRIC_PRESENTATION_REPRESENTATION (  '', ( #17365 ), #16986 ) ;
#4215 = CARTESIAN_POINT ( 'NONE',  ( 4.170895651974850793, 2.054890354522583618, -3.559174498016392185 ) ) ;
#4216 = B_SPLINE_CURVE_WITH_KNOTS ( 'NONE', 3,
 ( #17892, #19775, #10821, #14245, #7312, #10924, #18012, #14351 ),
 .UNSPECIFIED., .F., .F.,
 ( 4, 2, 2, 4 ),
 ( 0.002775112046897009431, 0.003466237704215413898, 0.004157363361533818365, 0.005539614676170626431 ),
 .UNSPECIFIED. ) ;
#4217 = AXIS2_PLACEMENT_3D ( 'NONE', #5709, #9805, #13341 ) ;
#4218 = ORIENTED_EDGE ( 'NONE', *, *, #16575, .F. ) ;
#4219 = CIRCLE ( 'NONE', #15511, 0.4999999999999995559 ) ;
#4220 = CIRCLE ( 'NONE', #118, 0.5000000000000004441 ) ;
#4222 = ORIENTED_EDGE ( 'NONE', *, *, #14818, .F. ) ;
#4221 = ORIENTED_EDGE ( 'NONE', *, *, #20349, .T. ) ;
#4223 = CARTESIAN_POINT ( 'NONE',  ( 0.000000000000000000, 0.000000000000000000, 0.000000000000000000 ) ) ;
#4224 = LINE ( 'NONE', #1185, #22748 ) ;
#4225 = ORIENTED_EDGE ( 'NONE', *, *, #22624, .T. ) ;
#4226 = CARTESIAN_POINT ( 'NONE',  ( -65.47859922179029013, -0.5000000000000628386, -11.38422848940298593 ) ) ;
#4227 = DIRECTION ( 'NONE',  ( 1.066786462891689527E-26, 6.656013887802287108E-31, 1.000000000000000000 ) ) ;
#4228 = CARTESIAN_POINT ( 'NONE',  ( 4.071447262713884463, -2.020725942163688504, 3.499999999999997780 ) ) ;
#4229 = FACE_OUTER_BOUND ( 'NONE', #1355, .T. ) ;
#4230 = CARTESIAN_POINT ( 'NONE',  ( -0.3263565795980838957, 4.430380094434251959, -5.351519936624994145 ) ) ;
#4231 = AXIS2_PLACEMENT_3D ( 'NONE', #21434, #14004, #5301 ) ;
#4232 = VECTOR ( 'NONE', #839, 1000.000000000000114 ) ;
#4233 = CARTESIAN_POINT ( 'NONE',  ( -3.499999999708153453, 13.99999999900385106, -19.50000000000000355 ) ) ;
#4234 =( GEOMETRIC_REPRESENTATION_CONTEXT ( 3 ) GLOBAL_UNCERTAINTY_ASSIGNED_CONTEXT ( ( #2266 ) ) GLOBAL_UNIT_ASSIGNED_CONTEXT ( ( #14864, #286, #1921 ) ) REPRESENTATION_CONTEXT ( 'NONE', 'WORKASPACE' ) );
#4235 = DIRECTION ( 'NONE',  ( -0.7313537016191730133, 0.6819983600624958120, -5.924440990721418971E-17 ) ) ;
#4236 = ADVANCED_FACE ( 'NONE', ( #19210 ), #11932, .T. ) ;
#4237 = AXIS2_PLACEMENT_3D ( 'NONE', #3567, #12608, #11191 ) ;
#4238 = DIRECTION ( 'NONE',  ( -1.066786462891689527E-26, -6.656013887802287108E-31, -1.000000000000000000 ) ) ;
#4239 = CIRCLE ( 'NONE', #139, 0.5000000000000029976 ) ;
#4240 = DIRECTION ( 'NONE',  ( 7.395570986446975166E-31, 3.382522293539642681E-32, 1.000000000000000000 ) ) ;
#4241 = FACE_OUTER_BOUND ( 'NONE', #14857, .T. ) ;
#4242 = LINE ( 'NONE', #7902, #14224 ) ;
#4243 = CARTESIAN_POINT ( 'NONE',  ( 119.5756419024615838, -6.500000000000061284, -6.499999999999992006 ) ) ;
#4244 = EDGE_CURVE ( 'NONE', #18520, #6499, #15342, .T. ) ;
#4245 = ORIENTED_EDGE ( 'NONE', *, *, #12674, .F. ) ;
#4246 = DIRECTION ( 'NONE',  ( 0.5804539248959940112, 0.8142930928559054538, -3.124497593494754418E-16 ) ) ;
#4248 = EDGE_LOOP ( 'NONE', ( #4166, #3417, #4430, #8421 ) ) ;
#4247 = ORIENTED_EDGE ( 'NONE', *, *, #8981, .T. ) ;
#4249 = ORIENTED_EDGE ( 'NONE', *, *, #4767, .F. ) ;
#4250 =( BOUNDED_SURFACE ( )  B_SPLINE_SURFACE ( 3, 2, ( 
 ( #12237, #10719, #14258 ),
 ( #7324, #19904, #21673 ),
 ( #19547, #12475, #5553 ),
 ( #19425, #21560, #12719 ),
 ( #12600, #19785, #1886 ),
 ( #9070, #2243, #15046 ) ),
 .UNSPECIFIED., .F., .F., .T. ) 
 B_SPLINE_SURFACE_WITH_KNOTS ( ( 4, 2, 4 ),
 ( 3, 3 ),
 ( 0.02032853247518126225, 0.02278863295364821906, 0.02524873343211517240 ),
 ( 0.000000000000000000, 1.000000000000000000 ),
 .UNSPECIFIED. ) 
 GEOMETRIC_REPRESENTATION_ITEM ( )  RATIONAL_B_SPLINE_SURFACE ( (
 ( 1.000000000000000000, 0.8047781615896839602, 1.000000000000000000),
 ( 1.000000000000000000, 0.8123767586289271092, 1.000000000000000000),
 ( 1.000000000000000000, 0.8190662415564389232, 1.000000000000000000),
 ( 1.000000000000000000, 0.8192361015669027413, 1.000000000000000000),
 ( 1.000000000000000000, 0.8126135807103893605, 1.000000000000000000),
 ( 1.000000000000000000, 0.8047712338318578906, 1.000000000000000000) ) ) 
 REPRESENTATION_ITEM ( '' )  SURFACE ( )  );
#4252 = EDGE_LOOP ( 'NONE', ( #11944, #22444, #10596, #6155, #17967, #15044, #2300 ) ) ;
#4251 = EDGE_LOOP ( 'NONE', ( #18817, #5197, #13985, #2641 ) ) ;
#4253 = AXIS2_PLACEMENT_3D ( 'NONE', #12931, #9289, #12810 ) ;
#4254 = ORIENTED_EDGE ( 'NONE', *, *, #4622, .F. ) ;
#4255 = AXIS2_PLACEMENT_3D ( 'NONE', #70, #16383, #7467 ) ;
#4256 = CARTESIAN_POINT ( 'NONE',  ( -12.84999999999999964, -2.000000000000001776, 0.000000000000000000 ) ) ;
#4257 = CIRCLE ( 'NONE', #17817, 2.550000000000012701 ) ;
#4258 = ORIENTED_EDGE ( 'NONE', *, *, #11390, .T. ) ;
#4259 = AXIS2_PLACEMENT_3D ( 'NONE', #15399, #20841, #832 ) ;
#4260 = EDGE_LOOP ( 'NONE', ( #7396, #548, #11338, #11339 ) ) ;
#4261 = DIRECTION ( 'NONE',  ( -1.000000000000000000, -2.699383410053119644E-30, -3.330669073875432643E-16 ) ) ;
#4262 = EDGE_CURVE ( 'NONE', #9468, #19219, #9812, .T. ) ;
#4263 = PLANE ( 'NONE',  #10034 ) ;
#4264 = CARTESIAN_POINT ( 'NONE',  ( 31.55000000029185259, 16.99999999900385461, -29.00000000000000355 ) ) ;
#4265 = APPLICATION_CONTEXT ( 'automotive_design' ) ;
#4266 = CARTESIAN_POINT ( 'NONE',  ( -45.37157287525408833, -6.828427124746183630, -7.500000000000034639 ) ) ;
#4267 = CARTESIAN_POINT ( 'NONE',  ( -2.000000000000015543, -3.464101615137743728, -5.600000000000000533 ) ) ;
#4268 = DIRECTION ( 'NONE',  ( -0.000000000000000000, -0.000000000000000000, 1.000000000000000000 ) ) ;
#4269 = DIRECTION ( 'NONE',  ( -1.479114197289397792E-31, 1.000000000000000000, 1.224646799147352961E-16 ) ) ;
#4270 = LINE ( 'NONE', #649, #10666 ) ;
#4271 = DIRECTION ( 'NONE',  ( -1.000000000000000000, -2.168404344971017743E-16, 1.780660105995169760E-30 ) ) ;
#4272 = FACE_OUTER_BOUND ( 'NONE', #8748, .T. ) ;
#4273 = CIRCLE ( 'NONE', #9542, 3.500000000000004441 ) ;
#4274 = VECTOR ( 'NONE', #15899, 1000.000000000000000 ) ;
#4275 = DIRECTION ( 'NONE',  ( -9.121204216617949000E-31, -1.000000000000000000, 6.982962677686261977E-15 ) ) ;
#4276 = CARTESIAN_POINT ( 'NONE',  ( -5.786576545576798125, 13.89610628501159795, -28.41807078404934117 ) ) ;
#4277 = DIRECTION ( 'NONE',  ( -1.000000000000000000, 1.276756478318922922E-15, 1.333893503340774882E-15 ) ) ;
#4278 = ORIENTED_EDGE ( 'NONE', *, *, #7805, .T. ) ;
#4279 =( LENGTH_UNIT ( ) NAMED_UNIT ( * ) SI_UNIT ( .MILLI., .METRE. ) );
#4281 = VERTEX_POINT ( 'NONE', #20876 ) ;
#4280 = ORIENTED_EDGE ( 'NONE', *, *, #6444, .T. ) ;
#4282 = EDGE_LOOP ( 'NONE', ( #11115, #16347, #7593, #7423, #16946, #12824, #19390, #8814, #2392 ) ) ;
#4283 = VERTEX_POINT ( 'NONE', #10044 ) ;
#4284 = ORIENTED_EDGE ( 'NONE', *, *, #9354, .F. ) ;
#4285 = ADVANCED_FACE ( 'NONE', ( #3105 ), #4407, .T. ) ;
#4286 = ORIENTED_EDGE ( 'NONE', *, *, #7371, .F. ) ;
#4287 = CARTESIAN_POINT ( 'NONE',  ( 111.3116192909783990, -9.818697260249948044, 6.000000000000074607 ) ) ;
#4288 = CIRCLE ( 'NONE', #2417, 0.7500000000000006661 ) ;
#4289 = CLOSED_SHELL ( 'NONE', ( #8465, #9973, #6985, #8602, #19738, #3770, #13689, #1432, #21243, #4960, #22507, #1018, #23037, #11307, #2466, #17849, #12289, #11838, #13259, #2732, #22595, #14500, #13541, #13166, #21733, #297, #11117, #12596, #17295, #12566, #20377, #13022, #11507, #7199, #3902, #4908, #1068, #11451, #19510, #7512, #14634, #16823, #15723, #2919, #6579, #9106, #7656, #2691, #12104, #15366, #3636, #21669, #14293, #7936, #14619, #17254, #3094, #19730, #5205, #3003, #15499, #13048, #16557, #12389, #13127, #22608, #11951, #12859, #5337, #10727, #22886, #19996, #12826, #12061, #4769 ) ) ;
#4290 = CARTESIAN_POINT ( 'NONE',  ( -91.14322581977724269, -0.5000000000001045830, 6.823838874241872077 ) ) ;
#4291 = VERTEX_POINT ( 'NONE', #2989 ) ;
#4292 = CARTESIAN_POINT ( 'NONE',  ( 82.19834661797897013, -6.499999999999811706, 6.000000000000109246 ) ) ;
#4293 = FACE_OUTER_BOUND ( 'NONE', #14730, .T. ) ;
#4294 = DIRECTION ( 'NONE',  ( 0.000000000000000000, 0.000000000000000000, 1.000000000000000000 ) ) ;
#4295 = DIRECTION ( 'NONE',  ( -1.000000000000000000, -3.254448077276381206E-32, -1.066788928082016908E-26 ) ) ;
#4296 = CARTESIAN_POINT ( 'NONE',  ( -7.972478112619585389, -12.36350260656811528, 7.628219499134346826 ) ) ;
#4297 = SHAPE_REPRESENTATION ( 'hex flange bolt small_iso_ISO 4162 - M5 x 25 x 16-N', ( #22115 ), #17228 ) ;
#4298 = CARTESIAN_POINT ( 'NONE',  ( -8.178874953434455364, -13.99214848402183087, 6.644730819939131727 ) ) ;
#4299 = CARTESIAN_POINT ( 'NONE',  ( -2.700000000000091216, -6.938893903907228378E-14, 7.500000000000117240 ) ) ;
#4300 = CARTESIAN_POINT ( 'NONE',  ( 66.26395429947837101, -4.500000000000003553, -5.999999999999956479 ) ) ;
#4301 = DIRECTION ( 'NONE',  ( 0.000000000000000000, 0.000000000000000000, 1.000000000000000000 ) ) ;
#4302 = STYLED_ITEM ( 'NONE', ( #22247 ), #19798 ) ;
#4303 = CARTESIAN_POINT ( 'NONE',  ( 2.775557561562891351E-14, 2.499999999999998668, -6.499999999999950262 ) ) ;
#4304 = CARTESIAN_POINT ( 'NONE',  ( 3.880198502136892547, 0.7307680362926917139, -3.500000000000009770 ) ) ;
#4305 = ORIENTED_EDGE ( 'NONE', *, *, #5455, .F. ) ;
#4306 = EDGE_CURVE ( 'NONE', #12775, #20034, #6104, .T. ) ;
#4307 = ORIENTED_EDGE ( 'NONE', *, *, #14528, .F. ) ;
#4308 = ORIENTED_EDGE ( 'NONE', *, *, #11113, .F. ) ;
#4309 = ORIENTED_EDGE ( 'NONE', *, *, #2900, .F. ) ;
#4310 = VERTEX_POINT ( 'NONE', #8047 ) ;
#4311 = EDGE_CURVE ( 'NONE', #5959, #11179, #18690, .T. ) ;
#4312 = FACE_OUTER_BOUND ( 'NONE', #5724, .T. ) ;
#4313 = CARTESIAN_POINT ( 'NONE',  ( 88.75737332930597745, -13.52760560296348302, -6.000000000000039968 ) ) ;
#4314 = ORIENTED_EDGE ( 'NONE', *, *, #3651, .T. ) ;
#4315 = DIRECTION ( 'NONE',  ( 1.000000000000000000, 1.479114197289397135E-31, 5.916456789157588541E-31 ) ) ;
#4316 = CARTESIAN_POINT ( 'NONE',  ( 1.387778780781445676E-14, 4.857225732735059864E-14, -1.500000000000001332 ) ) ;
#4317 = FACE_OUTER_BOUND ( 'NONE', #7342, .T. ) ;
#4318 = EDGE_CURVE ( 'NONE', #19103, #1910, #17947, .T. ) ;
#4319 = DIRECTION ( 'NONE',  ( -1.000000000000000000, 1.598721155460238356E-14, -3.717264591378832268E-16 ) ) ;
#4320 = CARTESIAN_POINT ( 'NONE',  ( 0.000000000000000000, 0.000000000000000000, -5.574599999999999334 ) ) ;
#4321 = EDGE_CURVE ( 'NONE', #4634, #7123, #7928, .T. ) ;
#4322 = CARTESIAN_POINT ( 'NONE',  ( 4.690415759823415520, 0.7500000000000700551, -2.000000000000001776 ) ) ;
#4323 = EDGE_CURVE ( 'NONE', #18414, #10626, #16965, .T. ) ;
#4324 = FACE_OUTER_BOUND ( 'NONE', #14131, .T. ) ;
#4325 = CARTESIAN_POINT ( 'NONE',  ( 124.5000000000017195, -4.500000000000059508, 1.387778780781445676E-14 ) ) ;
#4326 = DIRECTION ( 'NONE',  ( 0.4472135954999523766, 0.7745966692414836263, -0.4472135954999632568 ) ) ;
#4327 = CARTESIAN_POINT ( 'NONE',  ( -87.15000000000057412, -9.060110299520994546E-14, -2.000000000000002220 ) ) ;
#4328 = CARTESIAN_POINT ( 'NONE',  ( 4.071447262713884463, -2.020725942163695166, -3.500000000000000444 ) ) ;
#4329 = CARTESIAN_POINT ( 'NONE',  ( -5.551115123125782702E-14, 4.618802153517065356, -0.5000000000000004441 ) ) ;
#4330 = CARTESIAN_POINT ( 'NONE',  ( 4.052424581287676908, -3.786734753435080147, -0.5771415817957217254 ) ) ;
#4331 = ADVANCED_FACE ( 'NONE', ( #15332 ), #22632, .F. ) ;
#4332 = EDGE_CURVE ( 'NONE', #5138, #3763, #11137, .T. ) ;
#4333 = ORIENTED_EDGE ( 'NONE', *, *, #20748, .T. ) ;
#4335 = ORIENTED_EDGE ( 'NONE', *, *, #5254, .T. ) ;
#4334 = ORIENTED_EDGE ( 'NONE', *, *, #11549, .T. ) ;
#4336 = EDGE_CURVE ( 'NONE', #22242, #283, #17673, .T. ) ;
#4337 = CARTESIAN_POINT ( 'NONE',  ( 88.75737332930587797, -10.52760560296347947, 6.500000000000075495 ) ) ;
#4338 = EDGE_CURVE ( 'NONE', #7712, #12541, #22834, .T. ) ;
#4339 = FACE_OUTER_BOUND ( 'NONE', #9594, .T. ) ;
#4340 = MECHANICAL_DESIGN_GEOMETRIC_PRESENTATION_REPRESENTATION (  '', ( #22773 ), #12617 ) ;
#4341 = FACE_OUTER_BOUND ( 'NONE', #7364, .T. ) ;
#4343 = VERTEX_POINT ( 'NONE', #3346 ) ;
#4342 = EDGE_CURVE ( 'NONE', #16028, #6492, #10434, .T. ) ;
#4344 = LINE ( 'NONE', #2475, #7189 ) ;
#4345 = EDGE_CURVE ( 'NONE', #18159, #10396, #12611, .T. ) ;
#4346 = DIRECTION ( 'NONE',  ( 1.000000000000000000, 0.000000000000000000, 0.000000000000000000 ) ) ;
#4347 = CARTESIAN_POINT ( 'NONE',  ( -5.784122180648307854, 36.25568647312940840, -16.58536362057690638 ) ) ;
#4348 =( NAMED_UNIT ( * ) PLANE_ANGLE_UNIT ( ) SI_UNIT ( $, .RADIAN. ) );
#4349 = DIRECTION ( 'NONE',  ( 1.000000000000000000, 1.479114197289388027E-30, -2.013525853228518840E-32 ) ) ;
#4350 = CARTESIAN_POINT ( 'NONE',  ( -0.6554360035617893265, 4.240386000424037682, -0.1586754815284909248 ) ) ;
#4351 = DIRECTION ( 'NONE',  ( -1.756300210255732376E-61, 4.190823558986625216E-31, 1.000000000000000000 ) ) ;
#4352 = SURFACE_STYLE_FILL_AREA ( #11195 ) ;
#4354 = TOROIDAL_SURFACE ( 'NONE', #23166, 5.200000000000001066, 0.4999999999999978351 ) ;
#4353 = CARTESIAN_POINT ( 'NONE',  ( -90.55603112840533697, 3.200000000000057021, -7.432974388601714999 ) ) ;
#4355 = PLANE ( 'NONE',  #17557 ) ;
#4356 = CARTESIAN_POINT ( 'NONE',  ( -4.000000000000058620, -2.309401076758546445, -3.433295621305388678 ) ) ;
#4357 = DIRECTION ( 'NONE',  ( -1.000000000000000000, -5.598259082250514647E-17, -3.330669073875432643E-16 ) ) ;
#4358 = EDGE_LOOP ( 'NONE', ( #21641, #15913, #7147, #11232 ) ) ;
#4359 = AXIS2_PLACEMENT_3D ( 'NONE', #15235, #19128, #6435 ) ;
#4360 = EDGE_CURVE ( 'NONE', #6874, #19780, #10615, .T. ) ;
#4362 = ORIENTED_EDGE ( 'NONE', *, *, #197, .F. ) ;
#4361 = ORIENTED_EDGE ( 'NONE', *, *, #10211, .F. ) ;
#4363 = UNCERTAINTY_MEASURE_WITH_UNIT (LENGTH_MEASURE( 1.000000000000000082E-05 ), #14466, 'distance_accuracy_value', 'NONE');
#4364 = EDGE_LOOP ( 'NONE', ( #15796, #512, #16491, #17960 ) ) ;
#4365 = ORIENTED_EDGE ( 'NONE', *, *, #20832, .T. ) ;
#4367 = ORIENTED_EDGE ( 'NONE', *, *, #13056, .F. ) ;
#4366 = VERTEX_POINT ( 'NONE', #6746 ) ;
#4368 = ORIENTED_EDGE ( 'NONE', *, *, #2209, .T. ) ;
#4369 = EDGE_CURVE ( 'NONE', #2097, #9299, #3322, .T. ) ;
#4370 = CARTESIAN_POINT ( 'NONE',  ( 5.213674118230995802, -0.7499999999999382716, -1.500000000000001332 ) ) ;
#4371 = LINE ( 'NONE', #10032, #22350 ) ;
#4372 = EDGE_LOOP ( 'NONE', ( #398, #20998, #14486, #5957 ) ) ;
#4373 = CARTESIAN_POINT ( 'NONE',  ( 4.330127018922088844, -1.387778780781445676E-13, 7.500000000000027534 ) ) ;
#4374 = CIRCLE ( 'NONE', #2876, 2.500000000000002220 ) ;
#4375 = DIRECTION ( 'NONE',  ( 0.000000000000000000, 6.802837160693368935E-15, 1.000000000000000000 ) ) ;
#4376 = CARTESIAN_POINT ( 'NONE',  ( 0.000000000000000000, 0.000000000000000000, -0.2800830152838856835 ) ) ;
#4377 = CARTESIAN_POINT ( 'NONE',  ( 5.599999999999994316, 2.020725942163688504, -3.500000000000005773 ) ) ;
#4378 = CIRCLE ( 'NONE', #19799, 2.550000000000003819 ) ;
#4379 = AXIS2_PLACEMENT_3D ( 'NONE', #9322, #16480, #5806 ) ;
#4380 = DIRECTION ( 'NONE',  ( -1.000000000000000000, -3.254448077276381206E-32, -1.066788928082016908E-26 ) ) ;
#4381 = CARTESIAN_POINT ( 'NONE',  ( 3.345653888883671989, -2.687187980154742473, -5.460849780464843484 ) ) ;
#4382 = DIRECTION ( 'NONE',  ( -1.000000000000000000, -1.479114197289388027E-30, 2.013525853228518840E-32 ) ) ;
#4383 = AXIS2_PLACEMENT_3D ( 'NONE', #22868, #19919, #11074 ) ;
#4384 = CARTESIAN_POINT ( 'NONE',  ( -2.500000000000000000, 2.761527815601788505E-14, 17.24999999999997513 ) ) ;
#4385 = CARTESIAN_POINT ( 'NONE',  ( 22.50000000000003908, 4.500000000000031974, -0.2499999999999967526 ) ) ;
#4386 = AXIS2_PLACEMENT_3D ( 'NONE', #10331, #6585, #17030 ) ;
#4387 = CARTESIAN_POINT ( 'NONE',  ( 108.2426266706970637, -11.02760560296348125, 6.500000000000019540 ) ) ;
#4388 = CARTESIAN_POINT ( 'NONE',  ( 66.26395429947838522, 0.000000000000000000, 6.500000000000144773 ) ) ;
#4389 = CARTESIAN_POINT ( 'NONE',  ( 4.180232103119974063, 2.085387772176683807, -3.570466442734705481 ) ) ;
#4390 = PRODUCT_DEFINITION_SHAPE ( 'NONE', 'NONE',  #15220 ) ;
#4391 = ORIENTED_EDGE ( 'NONE', *, *, #14279, .T. ) ;
#4392 =( BOUNDED_SURFACE ( )  B_SPLINE_SURFACE ( 3, 2, ( 
 ( #9071, #9308, #18368 ),
 ( #10940, #602, #16230 ),
 ( #254, #11064, #18132 ),
 ( #5788, #22007, #9195 ),
 ( #2355, #16353, #7431 ),
 ( #16469, #18249, #21789 ),
 ( #9540, #16694, #7765 ),
 ( #9425, #5672, #10837 ) ),
 .UNSPECIFIED., .F., .F., .F. ) 
 B_SPLINE_SURFACE_WITH_KNOTS ( ( 4, 2, 2, 4 ),
 ( 3, 3 ),
 ( 3.665191429188093597, 3.926990816987242283, 4.188790204786391413, 4.712388980384689674 ),
 ( 0.000000000000000000, 1.000000000000000000 ),
 .UNSPECIFIED. ) 
 GEOMETRIC_REPRESENTATION_ITEM ( )  RATIONAL_B_SPLINE_SURFACE ( (
 ( 1.000000000000000000, 0.7905694150421759270, 1.000000000000000000),
 ( 1.000000000000000000, 0.8144940154005636535, 1.000000000000000000),
 ( 1.000000000000000000, 0.8408337562111811714, 1.000000000000000000),
 ( 1.000000000000000000, 0.8912170513578138165, 1.000000000000000000),
 ( 1.000000000000000000, 0.9152160911082614092, 1.000000000000000000),
 ( 1.000000000000000000, 0.9758108578640474207, 1.000000000000000000),
 ( 1.000000000000000000, 1.000509427570048571, 1.000000000000000000),
 ( 1.000000000000000000, 1.000000000000000000, 1.000000000000000000) ) ) 
 REPRESENTATION_ITEM ( '' )  SURFACE ( )  );
#4393 = CIRCLE ( 'NONE', #17545, 0.5000000000000004441 ) ;
#4395 = ORIENTED_EDGE ( 'NONE', *, *, #2261, .T. ) ;
#4394 = ORIENTED_EDGE ( 'NONE', *, *, #16257, .F. ) ;
#4396 = AXIS2_PLACEMENT_3D ( 'NONE', #17120, #20805, #17241 ) ;
#4397 = VERTEX_POINT ( 'NONE', #10850 ) ;
#4398 = EDGE_CURVE ( 'NONE', #7856, #9447, #5573, .T. ) ;
#4399 = ORIENTED_EDGE ( 'NONE', *, *, #19458, .F. ) ;
#4400 = VERTEX_POINT ( 'NONE', #6865 ) ;
#4401 = EDGE_CURVE ( 'NONE', #18942, #15314, #21461, .T. ) ;
#4402 = ORIENTED_EDGE ( 'NONE', *, *, #817, .T. ) ;
#4403 = CARTESIAN_POINT ( 'NONE',  ( 4.124214193018072905, -2.028338413290942110, 3.513185186763558843 ) ) ;
#4404 = VECTOR ( 'NONE', #18043, 1000.000000000000000 ) ;
#4405 = CARTESIAN_POINT ( 'NONE',  ( -8.660254037844406838, 0.000000000000000000, 6.938893903907228378E-15 ) ) ;
#4406 = ORIENTED_EDGE ( 'NONE', *, *, #1271, .F. ) ;
#4407 = CONICAL_SURFACE ( 'NONE', #4807, 4.750000000000000000, 1.047197551196600074 ) ;
#4408 = ADVANCED_FACE ( 'NONE', ( #13916 ), #21102, .F. ) ;
#4409 = FACE_OUTER_BOUND ( 'NONE', #15968, .T. ) ;
#4410 = CARTESIAN_POINT ( 'NONE',  ( 4.142654963991848405, 2.035398498734347417, 3.525413613457328843 ) ) ;
#4411 = FACE_OUTER_BOUND ( 'NONE', #3110, .T. ) ;
#4412 = AXIS2_PLACEMENT_3D ( 'NONE', #19853, #10897, #18090 ) ;
#4413 = CARTESIAN_POINT ( 'NONE',  ( 2.499999999999992006, 2.000000000000001776, -3.469446951953614189E-14 ) ) ;
#4414 = CARTESIAN_POINT ( 'NONE',  ( -8.498922697886669653, -12.49080420435820926, 6.997949321565080538 ) ) ;
#4415 = VECTOR ( 'NONE', #19101, 1000.000000000000000 ) ;
#4416 = CARTESIAN_POINT ( 'NONE',  ( 119.5756419024615553, -4.500000000000003553, 6.000000000000136779 ) ) ;
#4417 = CARTESIAN_POINT ( 'NONE',  ( 37.00000000000014211, 0.000000000000000000, -3.000000000000002665 ) ) ;
#4418 = CARTESIAN_POINT ( 'NONE',  ( 0.000000000000000000, 3.031088913245536087, 1.750000000000003331 ) ) ;
#4419 = CIRCLE ( 'NONE', #2923, 2.550000000000010481 ) ;
#4420 = CARTESIAN_POINT ( 'NONE',  ( 0.000000000000000000, 0.000000000000000000, 3.469446951953614189E-15 ) ) ;
#4422 = EDGE_CURVE ( 'NONE', #14933, #2848, #6268, .T. ) ;
#4421 = ORIENTED_EDGE ( 'NONE', *, *, #11242, .T. ) ;
#4423 = AXIS2_PLACEMENT_3D ( 'NONE', #19535, #21437, #1662 ) ;
#4424 =( NAMED_UNIT ( * ) PLANE_ANGLE_UNIT ( ) SI_UNIT ( $, .RADIAN. ) );
#4425 = CARTESIAN_POINT ( 'NONE',  ( 4.180231891692618440, 2.049421325483208545, 3.591231015387279957 ) ) ;
#4426 = CYLINDRICAL_SURFACE ( 'NONE', #10424, 0.5000000000000025535 ) ;
#4427 = ORIENTED_EDGE ( 'NONE', *, *, #11745, .F. ) ;
#4428 = B_SPLINE_CURVE_WITH_KNOTS ( 'NONE', 3,
 ( #8050, #16967, #22403, #22520, #20878, #880 ),
 .UNSPECIFIED., .F., .F.,
 ( 4, 2, 4 ),
 ( 0.004766700766612060741, 0.006150321146734550118, 0.007533941526857039495 ),
 .UNSPECIFIED. ) ;
#4429 = ORIENTED_EDGE ( 'NONE', *, *, #18037, .T. ) ;
#4430 = ORIENTED_EDGE ( 'NONE', *, *, #12114, .F. ) ;
#4431 = ORIENTED_EDGE ( 'NONE', *, *, #8397, .F. ) ;
#4432 = VERTEX_POINT ( 'NONE', #21345 ) ;
#4433 = COLOUR_RGB ( '', 0.40784314, 0.44705882, 0.49803922) ;
#4434 = CARTESIAN_POINT ( 'NONE',  ( -90.55603112840530855, 0.5000000000000490719, -7.432974388601742533 ) ) ;
#4435 = DIRECTION ( 'NONE',  ( 1.454462294001240516E-30, 1.000000000000000000, 0.000000000000000000 ) ) ;
#4436 = EDGE_LOOP ( 'NONE', ( #22147, #13709, #1581, #1038 ) ) ;
#4437 = CARTESIAN_POINT ( 'NONE',  ( 66.26395429947837101, -6.500000000000005329, -5.999999999999956479 ) ) ;
#4438 = CARTESIAN_POINT ( 'NONE',  ( 4.000000000000003553, 0.000000000000000000, -5.600000000000000533 ) ) ;
#4439 = SHAPE_REPRESENTATION ( 'hex flange bolt small_iso_ISO 4162 - M5 x 20 x 20-N', ( #22115 ), #2577 ) ;
#4440 = DIRECTION ( 'NONE',  ( -1.000000000000000000, 1.703746271048639119E-15, 0.000000000000000000 ) ) ;
#4441 = VECTOR ( 'NONE', #20804, 1000.000000000000000 ) ;
#4442 = DIRECTION ( 'NONE',  ( -2.220446049250313081E-16, 1.000000000000000000, -7.025792437124636392E-31 ) ) ;
#4443 = AXIS2_PLACEMENT_3D ( 'NONE', #468, #2458, #15037 ) ;
#4444 = DIRECTION ( 'NONE',  ( 0.9878135252003127365, -1.532010627492774434E-16, -0.1556420233463029767 ) ) ;
#4445 = AXIS2_PLACEMENT_3D ( 'NONE', #12636, #10757, #6890 ) ;
#4446 = CARTESIAN_POINT ( 'NONE',  ( 66.26395429947837101, -6.500000000000005329, 6.500000000000110134 ) ) ;
#4447 = FACE_OUTER_BOUND ( 'NONE', #13813, .T. ) ;
#4448 = PRODUCT_DEFINITION ( 'UNKNOWN', '', #15765, #1125 ) ;
#4449 = CARTESIAN_POINT ( 'NONE',  ( 0.000000000000000000, 2.999999999999992450, 0.000000000000000000 ) ) ;
#4450 = DIRECTION ( 'NONE',  ( 1.000000000000000000, 0.000000000000000000, 0.000000000000000000 ) ) ;
#4451 = DIRECTION ( 'NONE',  ( -0.7071067811865490160, -0.7071067811865460184, -1.565905175853766674E-16 ) ) ;
#4452 = CARTESIAN_POINT ( 'NONE',  ( -65.47859922179024750, -2.700000000000091216, -11.38422848940306942 ) ) ;
#4453 = DIRECTION ( 'NONE',  ( 1.000000000000000000, 2.168404344970991858E-16, -9.035018104045799943E-16 ) ) ;
#4454 = EDGE_CURVE ( 'NONE', #9571, #5465, #16022, .T. ) ;
#4455 = CARTESIAN_POINT ( 'NONE',  ( -12.84999999999999964, -12.00000000000011191, -5.749999999999963585 ) ) ;
#4456 = ORIENTED_EDGE ( 'NONE', *, *, #12037, .F. ) ;
#4457 = CONICAL_SURFACE ( 'NONE', #22900, 4.750000000000000888, 1.047197551196600074 ) ;
#4458 = EDGE_CURVE ( 'NONE', #14358, #7123, #16768, .T. ) ;
#4459 = ORIENTED_EDGE ( 'NONE', *, *, #14111, .T. ) ;
#4460 = B_SPLINE_CURVE_WITH_KNOTS ( 'NONE', 3,
 ( #15057, #22250, #13315, #4350, #18715, #387 ),
 .UNSPECIFIED., .F., .F.,
 ( 4, 2, 4 ),
 ( 0.002336974151641528670, 0.003500975885716446721, 0.004664977619791364771 ),
 .UNSPECIFIED. ) ;
#4461 = EDGE_CURVE ( 'NONE', #12152, #20279, #1688, .T. ) ;
#4463 = ORIENTED_EDGE ( 'NONE', *, *, #18024, .F. ) ;
#4462 = ORIENTED_EDGE ( 'NONE', *, *, #8114, .F. ) ;
#4464 = DIRECTION ( 'NONE',  ( 2.775557561562885188E-17, 1.309377075419427801E-16, 1.000000000000000000 ) ) ;
#4465 =( GEOMETRIC_REPRESENTATION_CONTEXT ( 3 ) GLOBAL_UNCERTAINTY_ASSIGNED_CONTEXT ( ( #14758 ) ) GLOBAL_UNIT_ASSIGNED_CONTEXT ( ( #9214, #11204, #7341 ) ) REPRESENTATION_CONTEXT ( 'NONE', 'WORKASPACE' ) );
#4466 = CARTESIAN_POINT ( 'NONE',  ( 2.742413778650823364, -1.325747111984059590, -4.750000000000000888 ) ) ;
#4467 = FACE_OUTER_BOUND ( 'NONE', #23244, .T. ) ;
#4468 = VERTEX_POINT ( 'NONE', #10735 ) ;
#4469 = LINE ( 'NONE', #21898, #3332 ) ;
#4470 = DIRECTION ( 'NONE',  ( 1.387778780781445676E-14, -1.000000000000000000, 0.000000000000000000 ) ) ;
#4471 = DIRECTION ( 'NONE',  ( -1.000000000000000000, -1.479114197289387852E-30, 2.013525853228518840E-32 ) ) ;
#4473 = EDGE_CURVE ( 'NONE', #22681, #9370, #22052, .T. ) ;
#4472 = CARTESIAN_POINT ( 'NONE',  ( -3.999999999708153453, 38.99999999900385461, -29.00000000000000355 ) ) ;
#4474 = CIRCLE ( 'NONE', #17627, 0.5000000000000031086 ) ;
#4475 = CARTESIAN_POINT ( 'NONE',  ( -6.763542839912098701E-14, -4.647091401871226601, -3.572172305156534833 ) ) ;
#4476 = DIRECTION ( 'NONE',  ( 4.190823558986625216E-31, -1.000000000000000000, 4.190823558986625216E-31 ) ) ;
#4477 = AXIS2_PLACEMENT_3D ( 'NONE', #4072, #670, #1140 ) ;
#4478 = CARTESIAN_POINT ( 'NONE',  ( -2.678494666091062015, -3.072372537026391459, -5.565789719053451101 ) ) ;
#4479 = DIRECTION ( 'NONE',  ( 0.000000000000000000, -0.7453559924999264563, 0.6666666666666704044 ) ) ;
#4480 = CARTESIAN_POINT ( 'NONE',  ( -65.00000000000052580, 3.200000000000057021, 3.000000000000002665 ) ) ;
#4481 = EDGE_CURVE ( 'NONE', #396, #4924, #17145, .T. ) ;
#4482 = DIRECTION ( 'NONE',  ( 1.454462294001240516E-30, 1.000000000000000000, 0.000000000000000000 ) ) ;
#4483 = CARTESIAN_POINT ( 'NONE',  ( -4.000000000000100364, 2.309401076758546445, -3.433295621305381573 ) ) ;
#4484 = DIRECTION ( 'NONE',  ( -0.7071067811865475727, -0.7071067811865475727, 0.000000000000000000 ) ) ;
#4485 = PRODUCT_DEFINITION_FORMATION_WITH_SPECIFIED_SOURCE ( 'ANY', '', #13808, .NOT_KNOWN. ) ;
#4486 = ORIENTED_EDGE ( 'NONE', *, *, #10023, .F. ) ;
#4487 = ADVANCED_FACE ( 'NONE', ( #17921 ), #15668, .F. ) ;
#4488 = EDGE_CURVE ( 'NONE', #17187, #5552, #23198, .T. ) ;
#4490 = ORIENTED_EDGE ( 'NONE', *, *, #18153, .T. ) ;
#4489 = EDGE_LOOP ( 'NONE', ( #2579, #1152, #8344, #18053 ) ) ;
#4491 = EDGE_CURVE ( 'NONE', #4310, #10913, #11145, .T. ) ;
#4492 = ORIENTED_EDGE ( 'NONE', *, *, #6913, .T. ) ;
#4494 = ORIENTED_EDGE ( 'NONE', *, *, #18247, .F. ) ;
#4493 = ORIENTED_EDGE ( 'NONE', *, *, #22019, .F. ) ;
#4495 = ORIENTED_EDGE ( 'NONE', *, *, #8640, .T. ) ;
#4496 = CARTESIAN_POINT ( 'NONE',  ( -2.081668171172168513E-14, 1.250000000000001110, 0.000000000000000000 ) ) ;
#4497 = DIRECTION ( 'NONE',  ( 0.000000000000000000, 0.000000000000000000, 1.000000000000000000 ) ) ;
#4498 = VERTEX_POINT ( 'NONE', #21687 ) ;
#4499 = AXIS2_PLACEMENT_3D ( 'NONE', #7468, #1922, #11322 ) ;
#4500 = LINE ( 'NONE', #3720, #20165 ) ;
#4501 = EDGE_CURVE ( 'NONE', #17483, #16256, #7033, .T. ) ;
#4502 = CARTESIAN_POINT ( 'NONE',  ( 1.387778780781445676E-14, 4.857225732735059864E-14, -1.500000000000001332 ) ) ;
#4503 = EDGE_CURVE ( 'NONE', #4023, #21589, #2429, .T. ) ;
#4504 = DIRECTION ( 'NONE',  ( 1.000000000000000000, 6.224605580259554159E-31, -2.887593071917436153E-31 ) ) ;
#4505 = CARTESIAN_POINT ( 'NONE',  ( 3.673643420401898840, 2.497823135841254150, -0.2484800633749945087 ) ) ;
#4506 = ADVANCED_FACE ( 'NONE', ( #389 ), #2133, .T. ) ;
#4507 = EDGE_CURVE ( 'NONE', #13843, #11516, #22812, .T. ) ;
#4508 = DIRECTION ( 'NONE',  ( -1.000000000000000000, -2.699383410053119644E-30, -3.330669073875432643E-16 ) ) ;
#4509 = CARTESIAN_POINT ( 'NONE',  ( 3.999999999999981792, 2.472263674411438128, -3.687027874309864561 ) ) ;
#4510 = CARTESIAN_POINT ( 'NONE',  ( 8.037202331403262789, -2.196591282338120621, 7.528743044528568795 ) ) ;
#4511 = LINE ( 'NONE', #22399, #538 ) ;
#4512 = CARTESIAN_POINT ( 'NONE',  ( 37.52451905283846401, 0.09150635094610139186, -2.816987298107726634 ) ) ;
#4513 = DIRECTION ( 'NONE',  ( -8.438582421954109416E-32, 0.000000000000000000, -1.000000000000000000 ) ) ;
#4514 = CARTESIAN_POINT ( 'NONE',  ( -45.37157287525418781, 6.828427124746204058, -8.000000000000035527 ) ) ;
#4515 = DIRECTION ( 'NONE',  ( 3.885780586188016830E-16, 4.437342591868156373E-31, -1.000000000000000000 ) ) ;
#4516 = EDGE_CURVE ( 'NONE', #17475, #3321, #20266, .T. ) ;
#4517 = CARTESIAN_POINT ( 'NONE',  ( 4.086375874528098251, -2.103253014742891391, -3.500000000000007105 ) ) ;
#4518 = ORIENTED_EDGE ( 'NONE', *, *, #19272, .F. ) ;
#4519 = ADVANCED_FACE ( 'NONE', ( #9323 ), #12845, .T. ) ;
#4520 = CONICAL_SURFACE ( 'NONE', #13908, 4.487534009422209813, 0.08726646259971666819 ) ;
#4522 = ORIENTED_EDGE ( 'NONE', *, *, #12794, .F. ) ;
#4521 = ORIENTED_EDGE ( 'NONE', *, *, #1932, .F. ) ;
#4523 = VERTEX_POINT ( 'NONE', #2371 ) ;
#4524 = EDGE_LOOP ( 'NONE', ( #2027, #10750, #3434 ) ) ;
#4525 = ORIENTED_EDGE ( 'NONE', *, *, #17435, .F. ) ;
#4526 = EDGE_LOOP ( 'NONE', ( #8030, #16492, #3764, #6612 ) ) ;
#4527 = CARTESIAN_POINT ( 'NONE',  ( 1.199999999999992628, -0.5999999999999963141, 4.543283425070391068 ) ) ;
#4528 = LINE ( 'NONE', #16875, #1259 ) ;
#4529 = ORIENTED_EDGE ( 'NONE', *, *, #10067, .F. ) ;
#4530 = ORIENTED_EDGE ( 'NONE', *, *, #16463, .F. ) ;
#4531 = DIRECTION ( 'NONE',  ( -1.333893503340774882E-15, -2.778352770573747380E-17, -1.000000000000000000 ) ) ;
#4532 = FACE_OUTER_BOUND ( 'NONE', #4699, .T. ) ;
#4533 = DIRECTION ( 'NONE',  ( -1.000000000000000000, -1.479114197289388027E-30, 2.013525853228518840E-32 ) ) ;
#4534 = DIRECTION ( 'NONE',  ( 1.000000000000000000, 2.172745813409351317E-17, 9.470910429910635790E-17 ) ) ;
#4535 = CIRCLE ( 'NONE', #4914, 2.500000000000002220 ) ;
#4536 = CARTESIAN_POINT ( 'NONE',  ( -10.49999999999998224, -12.00000000000002842, 5.750000000000018652 ) ) ;
#4537 = CARTESIAN_POINT ( 'NONE',  ( 4.158413352280815545, 4.089743253945648860, -1.734723475976807094E-15 ) ) ;
#4538 = CARTESIAN_POINT ( 'NONE',  ( -8.429621201837608879, -14.00000000000004619, 6.425428529985135917 ) ) ;
#4539 = DIRECTION ( 'NONE',  ( -1.000000000000000000, 0.000000000000000000, -1.613696256722611405E-16 ) ) ;
#4540 = DIRECTION ( 'NONE',  ( 1.000000000000000000, -4.440892098500655744E-16, 7.860214984770760936E-18 ) ) ;
#4541 = ADVANCED_FACE ( 'NONE', ( #7558 ), #16364, .F. ) ;
#4542 = DIRECTION ( 'NONE',  ( -0.000000000000000000, -0.000000000000000000, 1.000000000000000000 ) ) ;
#4543 = VERTEX_POINT ( 'NONE', #11196 ) ;
#4544 = CARTESIAN_POINT ( 'NONE',  ( 36.00000000029184832, 2.999999999003851503, 0.000000000000000000 ) ) ;
#4545 = CARTESIAN_POINT ( 'NONE',  ( 77.42435809754145737, -4.499999999999809930, -6.499999999999984901 ) ) ;
#4546 = VERTEX_POINT ( 'NONE', #14501 ) ;
#4547 = ADVANCED_FACE ( 'NONE', ( #18041 ), #13401, .T. ) ;
#4548 = EDGE_LOOP ( 'NONE', ( #22260, #9674, #11119, #9817 ) ) ;
#4549 = AXIS2_PLACEMENT_3D ( 'NONE', #20339, #2811, #4203 ) ;
#4550 =( GEOMETRIC_REPRESENTATION_CONTEXT ( 3 ) GLOBAL_UNCERTAINTY_ASSIGNED_CONTEXT ( ( #8145 ) ) GLOBAL_UNIT_ASSIGNED_CONTEXT ( ( #10644, #8890, #14301 ) ) REPRESENTATION_CONTEXT ( 'NONE', 'WORKASPACE' ) );
#4551 = ORIENTED_EDGE ( 'NONE', *, *, #11549, .F. ) ;
#4552 = PLANE ( 'NONE',  #9871 ) ;
#4553 = DIRECTION ( 'NONE',  ( -3.885780586188016830E-16, -4.437342591868156373E-31, 1.000000000000000000 ) ) ;
#4554 = ORIENTED_EDGE ( 'NONE', *, *, #20162, .T. ) ;
#4555 = CARTESIAN_POINT ( 'NONE',  ( 0.000000000000000000, 0.000000000000000000, 0.000000000000000000 ) ) ;
#4556 = DIRECTION ( 'NONE',  ( 0.7313537016191746787, 0.6819983600624940356, 1.072890437865584409E-16 ) ) ;
#4557 = CARTESIAN_POINT ( 'NONE',  ( -6.977878452303022172, 35.99999999900387593, -18.50953884562097684 ) ) ;
#4558 = CARTESIAN_POINT ( 'NONE',  ( 3.961551342854056745, 2.319461885623242292, 2.982574167880871485 ) ) ;
#4559 = CARTESIAN_POINT ( 'NONE',  ( -6.000000000000102141, 4.799999999999964295, 8.000000000000047962 ) ) ;
#4560 = CARTESIAN_POINT ( 'NONE',  ( 0.000000000000000000, 0.000000000000000000, 0.000000000000000000 ) ) ;
#4561 = LINE ( 'NONE', #20933, #13811 ) ;
#4562 = AXIS2_PLACEMENT_3D ( 'NONE', #11730, #21986, #2678 ) ;
#4563 = CARTESIAN_POINT ( 'NONE',  ( -5.773502691896256422, 5.000000000000003553, -4.999999999999975131 ) ) ;
#4564 = LINE ( 'NONE', #6234, #6291 ) ;
#4565 = LINE ( 'NONE', #19268, #8493 ) ;
#4566 = CARTESIAN_POINT ( 'NONE',  ( 2.775557561562891351E-14, 8.000000000000003553, -12.50000000000001066 ) ) ;
#4567 = VERTEX_POINT ( 'NONE', #9438 ) ;
#4568 = CONTEXT_DEPENDENT_SHAPE_REPRESENTATION ( #14652, #10620 ) ;
#4569 = VERTEX_POINT ( 'NONE', #16584 ) ;
#4571 = EDGE_LOOP ( 'NONE', ( #20283, #21646, #6979, #16063 ) ) ;
#4570 = ORIENTED_EDGE ( 'NONE', *, *, #12459, .T. ) ;
#4572 = AXIS2_PLACEMENT_3D ( 'NONE', #4011, #2019, #7669 ) ;
#4573 = ORIENTED_EDGE ( 'NONE', *, *, #4516, .F. ) ;
#4574 = DIRECTION ( 'NONE',  ( -2.172745813409349776E-17, 1.000000000000000000, -1.309377075419428048E-16 ) ) ;
#4575 = VECTOR ( 'NONE', #10673, 1000.000000000000000 ) ;
#4576 = DIRECTION ( 'NONE',  ( -1.000000000000000000, 1.550910762415513985E-16, 3.012982189080959477E-32 ) ) ;
#4577 = ADVANCED_FACE ( 'NONE', ( #7674 ), #1396, .T. ) ;
#4578 = LINE ( 'NONE', #7659, #22137 ) ;
#4579 = ORIENTED_EDGE ( 'NONE', *, *, #8393, .T. ) ;
#4580 = DIRECTION ( 'NONE',  ( 1.110223024625150131E-16, -1.000000000000000000, 6.902532920683853297E-31 ) ) ;
#4581 = CARTESIAN_POINT ( 'NONE',  ( 116.5066492821803052, -7.708908342713815642, -6.500000000000005329 ) ) ;
#4582 = PRODUCT_DEFINITION_SHAPE ( 'NONE', 'NONE',  #23275 ) ;
#4583 = CARTESIAN_POINT ( 'NONE',  ( -56.91911807125098477, -2.700000000000084110, -8.333333333333413862 ) ) ;
#4584 = DIRECTION ( 'NONE',  ( -0.000000000000000000, 1.000000000000000000, -0.000000000000000000 ) ) ;
#4585 = CARTESIAN_POINT ( 'NONE',  ( 2.775557561562891351E-14, 10.49999999999998579, -3.000000000000002665 ) ) ;
#4586 = VECTOR ( 'NONE', #12021, 1000.000000000000000 ) ;
#4587 = FACE_OUTER_BOUND ( 'NONE', #2997, .T. ) ;
#4588 = DIRECTION ( 'NONE',  ( -9.121204216617949000E-31, -1.000000000000000000, 6.982962677686261977E-15 ) ) ;
#4589 = LINE ( 'NONE', #6483, #1815 ) ;
#4590 = DIRECTION ( 'NONE',  ( -0.000000000000000000, -1.000000000000000000, -0.000000000000000000 ) ) ;
#4591 = DIRECTION ( 'NONE',  ( 1.333893503340774882E-15, 2.778352770573747380E-17, 1.000000000000000000 ) ) ;
#4592 = TOROIDAL_SURFACE ( 'NONE', #7611, 1.750000000000000000, 0.2500000000000000000 ) ;
#4593 = CARTESIAN_POINT ( 'NONE',  ( 0.000000000000000000, 0.000000000000000000, -5.600000000000000533 ) ) ;
#4595 = AXIS2_PLACEMENT_3D ( 'NONE', #14437, #21622, #7265 ) ;
#4594 = DIRECTION ( 'NONE',  ( 1.000000000000000000, 2.699383410053119644E-30, 3.330669073875432643E-16 ) ) ;
#4596 = CIRCLE ( 'NONE', #9884, 4.000000000000023981 ) ;
#4597 = ORIENTED_EDGE ( 'NONE', *, *, #11360, .T. ) ;
#4598 = AXIS2_PLACEMENT_3D ( 'NONE', #3850, #1970, #5637 ) ;
#4599 = FILL_AREA_STYLE ('',( #11542 ) ) ;
#4601 = ORIENTED_EDGE ( 'NONE', *, *, #18024, .T. ) ;
#4600 = EDGE_LOOP ( 'NONE', ( #12470, #7198, #22125, #11896 ) ) ;
#4602 = UNCERTAINTY_MEASURE_WITH_UNIT (LENGTH_MEASURE( 1.000000000000000082E-05 ), #19888, 'distance_accuracy_value', 'NONE');
#4603 = VERTEX_POINT ( 'NONE', #4121 ) ;
#4604 = ADVANCED_FACE ( 'NONE', ( #259 ), #20018, .T. ) ;
#4606 = VERTEX_POINT ( 'NONE', #11298 ) ;
#4605 = ORIENTED_EDGE ( 'NONE', *, *, #5254, .F. ) ;
#4607 = ORIENTED_EDGE ( 'NONE', *, *, #13156, .T. ) ;
#4608 = FACE_OUTER_BOUND ( 'NONE', #22785, .T. ) ;
#4609 = CYLINDRICAL_SURFACE ( 'NONE', #11062, 0.5000000000000038858 ) ;
#4610 = ADVANCED_FACE ( 'NONE', ( #4229 ), #18479, .T. ) ;
#4611 = AXIS2_PLACEMENT_3D ( 'NONE', #18710, #11642, #2592 ) ;
#4612 = CARTESIAN_POINT ( 'NONE',  ( 2.775557561562891351E-14, 7.999999999999983125, -0.4999999999999865663 ) ) ;
#4613 = AXIS2_PLACEMENT_3D ( 'NONE', #8528, #7010, #7134 ) ;
#4614 = CARTESIAN_POINT ( 'NONE',  ( 0.000000000000000000, 0.000000000000000000, 0.000000000000000000 ) ) ;
#4615 = AXIS2_PLACEMENT_3D ( 'NONE', #993, #762, #6050 ) ;
#4616 = DIRECTION ( 'NONE',  ( 0.000000000000000000, 0.000000000000000000, 1.000000000000000000 ) ) ;
#4617 = AXIS2_PLACEMENT_3D ( 'NONE', #1105, #2729, #13904 ) ;
#4618 = DIRECTION ( 'NONE',  ( 1.733449886265891589E-32, -4.190823558986610327E-31, 1.000000000000000000 ) ) ;
#4619 = EDGE_CURVE ( 'NONE', #5046, #9224, #14836, .T. ) ;
#4620 = CARTESIAN_POINT ( 'NONE',  ( 3.999999999999980904, 2.512223110932565007, -3.469391141908806819 ) ) ;
#4621 = DIRECTION ( 'NONE',  ( -1.000000000000000000, -2.699383410053119644E-30, -3.330669073875432643E-16 ) ) ;
#4622 = EDGE_CURVE ( 'NONE', #3142, #12159, #13354, .T. ) ;
#4623 = LINE ( 'NONE', #22983, #17035 ) ;
#4624 = CARTESIAN_POINT ( 'NONE',  ( 2.775557561562891351E-14, 8.000000000000003553, -12.99999999999999822 ) ) ;
#4625 = CARTESIAN_POINT ( 'NONE',  ( 37.00000000000011369, 11.00000000000000000, -10.00000000000000888 ) ) ;
#4626 = CARTESIAN_POINT ( 'NONE',  ( -10.49999999999999467, -12.00000000000000711, 9.250000000000021316 ) ) ;
#4627 = LINE ( 'NONE', #18868, #14946 ) ;
#4628 = CARTESIAN_POINT ( 'NONE',  ( 3.950233766685598447, 0.7256672287173716596, -3.500000000000161204 ) ) ;
#4629 = ORIENTED_EDGE ( 'NONE', *, *, #23195, .T. ) ;
#4630 = PRODUCT_DEFINITION_CONTEXT ( 'detailed design', #10732, 'design' ) ;
#4631 = AXIS2_PLACEMENT_3D ( 'NONE', #8571, #3626, #17621 ) ;
#4632 = FILL_AREA_STYLE ('',( #22526 ) ) ;
#4633 = AXIS2_PLACEMENT_3D ( 'NONE', #13285, #2570, #11501 ) ;
#4635 = EDGE_LOOP ( 'NONE', ( #10093, #2618, #1596, #22505 ) ) ;
#4634 = VERTEX_POINT ( 'NONE', #5900 ) ;
#4636 = VECTOR ( 'NONE', #22715, 1000.000000000000000 ) ;
#4637 = AXIS2_PLACEMENT_3D ( 'NONE', #20982, #8859, #21457 ) ;
#4638 = CIRCLE ( 'NONE', #20436, 4.750000000000013323 ) ;
#4639 = ORIENTED_EDGE ( 'NONE', *, *, #4114, .T. ) ;
#4640 = MECHANICAL_DESIGN_GEOMETRIC_PRESENTATION_REPRESENTATION (  '', ( #10654 ), #23062 ) ;
#4641 = EDGE_CURVE ( 'NONE', #20325, #12512, #12801, .T. ) ;
#4642 = EDGE_CURVE ( 'NONE', #22761, #4543, #9287, .T. ) ;
#4643 = ORIENTED_EDGE ( 'NONE', *, *, #184, .F. ) ;
#4644 = EDGE_LOOP ( 'NONE', ( #16117, #8849, #1006, #19831 ) ) ;
#4645 = ORIENTED_EDGE ( 'NONE', *, *, #15832, .T. ) ;
#4646 = CARTESIAN_POINT ( 'NONE',  ( 3.806834918298639625, 3.031088913245540528, -1.750000000000002442 ) ) ;
#4647 = DIRECTION ( 'NONE',  ( -5.551115123561405253E-17, -1.000000000000000000, -2.256980353643891447E-27 ) ) ;
#4648 = EDGE_CURVE ( 'NONE', #20913, #283, #1027, .T. ) ;
#4649 = VERTEX_POINT ( 'NONE', #2594 ) ;
#4650 = DIRECTION ( 'NONE',  ( -2.013525853228507892E-32, -6.902532920683810383E-31, 1.000000000000000000 ) ) ;
#4651 = CARTESIAN_POINT ( 'NONE',  ( 4.000000000000003553, 2.309401076758525573, -5.242734410091827613 ) ) ;
#4652 = TOROIDAL_SURFACE ( 'NONE', #2008, 5.200000000000001066, 0.4999999999999978351 ) ;
#4653 = EDGE_CURVE ( 'NONE', #15514, #6303, #1319, .T. ) ;
#4654 = CARTESIAN_POINT ( 'NONE',  ( 66.26395429947839943, 0.000000000000000000, 6.000000000000178524 ) ) ;
#4655 = VECTOR ( 'NONE', #1899, 1000.000000000000000 ) ;
#4656 = CARTESIAN_POINT ( 'NONE',  ( -2.700000000000091216, 1.999999999999946265, -7.500000000000034639 ) ) ;
#4657 = CARTESIAN_POINT ( 'NONE',  ( -4.330127018922234505, -2.775557561562891351E-14, -7.499999999999989342 ) ) ;
#4658 = AXIS2_PLACEMENT_3D ( 'NONE', #19034, #1043, #20455 ) ;
#4659 = FACE_OUTER_BOUND ( 'NONE', #16373, .T. ) ;
#4660 = ADVANCED_FACE ( 'NONE', ( #19504 ), #20558, .F. ) ;
#4661 = CARTESIAN_POINT ( 'NONE',  ( -8.496394830447192348, -13.96748264593578526, 6.998792816379799220 ) ) ;
#4662 = DIRECTION ( 'NONE',  ( 2.655250634480531216E-32, -6.902532920683810383E-31, 1.000000000000000000 ) ) ;
#4663 = CARTESIAN_POINT ( 'NONE',  ( 77.42435809754134368, -10.99999999999981526, -6.000000000000047073 ) ) ;
#4664 = DIRECTION ( 'NONE',  ( 2.013525853228507892E-32, 6.902532920683810383E-31, -1.000000000000000000 ) ) ;
#4665 = ORIENTED_EDGE ( 'NONE', *, *, #5939, .T. ) ;
#4666 =( LENGTH_UNIT ( ) NAMED_UNIT ( * ) SI_UNIT ( .MILLI., .METRE. ) );
#4667 = LINE ( 'NONE', #6208, #327 ) ;
#4668 = DIRECTION ( 'NONE',  ( 1.000000000000000000, 2.168404344971017743E-16, -1.780660105995169760E-30 ) ) ;
#4669 = ORIENTED_EDGE ( 'NONE', *, *, #18556, .T. ) ;
#4670 = AXIS2_PLACEMENT_3D ( 'NONE', #8858, #6990, #5325 ) ;
#4671 = VERTEX_POINT ( 'NONE', #3399 ) ;
#4672 = CLOSED_SHELL ( 'NONE', ( #11669, #7961, #492, #3669, #19798, #15997, #20730, #22456, #17874 ) ) ;
#4673 = VECTOR ( 'NONE', #13194, 1000.000000000000000 ) ;
#4674 = EDGE_LOOP ( 'NONE', ( #5669, #11410, #16266, #19571 ) ) ;
#4675 = ORIENTED_EDGE ( 'NONE', *, *, #13532, .F. ) ;
#4676 = AXIS2_PLACEMENT_3D ( 'NONE', #16270, #12629, #16497 ) ;
#4677 = ORIENTED_EDGE ( 'NONE', *, *, #6379, .T. ) ;
#4678 = CARTESIAN_POINT ( 'NONE',  ( -3.414274948570356294, 0.5000000000000628386, -21.66938530120590656 ) ) ;
#4679 = CARTESIAN_POINT ( 'NONE',  ( -6.938893903907228378E-14, -4.618802153517020059, -0.3572655899081733644 ) ) ;
#4680 = EDGE_LOOP ( 'NONE', ( #7094, #1812, #4864, #11174 ) ) ;
#4681 = DIRECTION ( 'NONE',  ( -1.000000000000000000, 1.424116703980815236E-16, 2.931272055834072749E-32 ) ) ;
#4682 = EDGE_CURVE ( 'NONE', #20043, #17223, #22435, .T. ) ;
#4683 = FACE_OUTER_BOUND ( 'NONE', #18648, .T. ) ;
#4684 = CARTESIAN_POINT ( 'NONE',  ( 2.107079159589796892E-14, -2.859595677584363393, 2.047034997319605143 ) ) ;
#4685 = CARTESIAN_POINT ( 'NONE',  ( -4.711587335155682510, 35.99999999900384751, -19.05331844708923938 ) ) ;
#4686 = FACE_OUTER_BOUND ( 'NONE', #18531, .T. ) ;
#4687 = B_SPLINE_CURVE_WITH_KNOTS ( 'NONE', 3,
 ( #5587, #17485, #1917, #5017, #3154, #21150, #14512, #10317, #3031, #21700, #1272, #10195, #1385, #9102, #12747, #8448 ),
 .UNSPECIFIED., .F., .F.,
 ( 4, 3, 3, 3, 3, 4 ),
 ( 0.000000000000000000, 3.315506744709155554E-05, 6.608280158698813327E-05, 0.0001026520855291343043, 0.0001376952025664795565, 0.0001398064759190610737 ),
 .UNSPECIFIED. ) ;
#4688 = CARTESIAN_POINT ( 'NONE',  ( -8.721922330811995749, -0.01237189218572515466, 6.818491697977000499 ) ) ;
#4689 = ADVANCED_FACE ( 'NONE', ( #2705 ), #5156, .T. ) ;
#4690 = CARTESIAN_POINT ( 'NONE',  ( 8.697224362267995446, -14.00000000000004974, 6.250000000000070166 ) ) ;
#4691 = CIRCLE ( 'NONE', #15943, 0.5000000000000028866 ) ;
#4692 = CARTESIAN_POINT ( 'NONE',  ( -47.47487373415315659, -4.018019484660608320, -8.000000000000007105 ) ) ;
#4693 = CIRCLE ( 'NONE', #11447, 6.700000000000039257 ) ;
#4694 = DIRECTION ( 'NONE',  ( -1.000000000000000000, 1.734723475976796001E-16, 0.000000000000000000 ) ) ;
#4695 = CARTESIAN_POINT ( 'NONE',  ( -7.500000000000020428, -1.390227771353544473, 9.250000000000008882 ) ) ;
#4696 = DIRECTION ( 'NONE',  ( 1.000000000000000000, 3.915518702919051914E-14, 0.000000000000000000 ) ) ;
#4697 = DIRECTION ( 'NONE',  ( 0.000000000000000000, 0.000000000000000000, -1.000000000000000000 ) ) ;
#4698 = ITEM_DEFINED_TRANSFORMATION ( 'NONE', 'NONE', #6384,  #22115 ) ;
#4699 = EDGE_LOOP ( 'NONE', ( #18157, #10187, #2908, #5615 ) ) ;
#4700 = B_SPLINE_CURVE_WITH_KNOTS ( 'NONE', 3,
 ( #12344, #16214, #21309, #15988, #11047, #12812 ),
 .UNSPECIFIED., .F., .F.,
 ( 4, 2, 4 ),
 ( 0.003358874760055556661, 0.004541967308452141486, 0.005725059856848725010 ),
 .UNSPECIFIED. ) ;
#4701 = AXIS2_PLACEMENT_3D ( 'NONE', #8456, #15616, #11503 ) ;
#4703 = ORIENTED_EDGE ( 'NONE', *, *, #4336, .F. ) ;
#4702 = ORIENTED_EDGE ( 'NONE', *, *, #20170, .F. ) ;
#4704 = VECTOR ( 'NONE', #14338, 1000.000000000000000 ) ;
#4705 = ORIENTED_EDGE ( 'NONE', *, *, #9638, .T. ) ;
#4706 = CARTESIAN_POINT ( 'NONE',  ( 31.55000000029185259, 16.99999999900385461, -19.00000000000000355 ) ) ;
#4707 = EDGE_CURVE ( 'NONE', #688, #690, #15838, .T. ) ;
#4708 = CARTESIAN_POINT ( 'NONE',  ( 2.775557561562891351E-14, 2.999999999999999112, -12.50000000000001066 ) ) ;
#4709 = CARTESIAN_POINT ( 'NONE',  ( 3.646393709166121599, -1.749999999999999556, -3.184260831324760233 ) ) ;
#4710 = ORIENTED_EDGE ( 'NONE', *, *, #11545, .F. ) ;
#4711 = DIRECTION ( 'NONE',  ( -1.000000000000000000, 4.615739097524200579E-16, 1.134196829589820086E-15 ) ) ;
#4712 = DIRECTION ( 'NONE',  ( -1.000000000000000000, 4.437342591868175641E-31, -3.330669073875457788E-16 ) ) ;
#4713 = EDGE_CURVE ( 'NONE', #5552, #18229, #4091, .T. ) ;
#4714 = CARTESIAN_POINT ( 'NONE',  ( 29.00000000029184832, 16.99999999900385461, -26.50000000000000000 ) ) ;
#4715 = CARTESIAN_POINT ( 'NONE',  ( 0.000000000000000000, 0.6000000000000137446, 3.054668707061600319 ) ) ;
#4716 = CARTESIAN_POINT ( 'NONE',  ( 84.32438398889955522, -11.28140466348809312, 6.000000000000095923 ) ) ;
#4717 = DIRECTION ( 'NONE',  ( 1.000000000000000000, 2.775557561562873996E-14, 1.768522514469825155E-30 ) ) ;
#4718 = CARTESIAN_POINT ( 'NONE',  ( -1.387778780781445676E-14, 2.000000000000001776, -2.000000000000001776 ) ) ;
#4719 = CARTESIAN_POINT ( 'NONE',  ( -64.00000000000045475, -7.632783294297951215E-14, -2.000000000000001776 ) ) ;
#4720 = DIRECTION ( 'NONE',  ( 0.000000000000000000, 0.000000000000000000, -1.000000000000000000 ) ) ;
#4721 = ORIENTED_EDGE ( 'NONE', *, *, #15102, .T. ) ;
#4722 = EDGE_CURVE ( 'NONE', #14397, #19077, #21323, .T. ) ;
#4723 = VECTOR ( 'NONE', #1109, 1000.000000000000000 ) ;
#4724 = CARTESIAN_POINT ( 'NONE',  ( -142.9465341061813035, 73.31261843211507312, 28.66570243528391515 ) ) ;
#4726 = ORIENTED_EDGE ( 'NONE', *, *, #5664, .T. ) ;
#4725 = ORIENTED_EDGE ( 'NONE', *, *, #8260, .T. ) ;
#4727 = ORIENTED_EDGE ( 'NONE', *, *, #8358, .T. ) ;
#4729 = ORIENTED_EDGE ( 'NONE', *, *, #6094, .T. ) ;
#4728 = ORIENTED_EDGE ( 'NONE', *, *, #1907, .T. ) ;
#4730 = B_SPLINE_CURVE_WITH_KNOTS ( 'NONE', 3,
 ( #14222, #14100, #6937, #9039, #14329, #1854 ),
 .UNSPECIFIED., .F., .F.,
 ( 4, 2, 4 ),
 ( 0.002365888236228012864, 0.003551327329835094089, 0.004736766423442174447 ),
 .UNSPECIFIED. ) ;
#4731 = DIRECTION ( 'NONE',  ( 1.000000000000000000, 1.479114197289388027E-30, -2.013525853228518840E-32 ) ) ;
#4732 = DIRECTION ( 'NONE',  ( 0.000000000000000000, 0.000000000000000000, 1.000000000000000000 ) ) ;
#4733 = DIRECTION ( 'NONE',  ( 3.032184104443271834E-30, 1.000000000000000000, 4.437342591868167759E-31 ) ) ;
#4734 = AXIS2_PLACEMENT_3D ( 'NONE', #10786, #13023, #3505 ) ;
#4735 = DIRECTION ( 'NONE',  ( 0.000000000000000000, 0.000000000000000000, 1.000000000000000000 ) ) ;
#4736 = CARTESIAN_POINT ( 'NONE',  ( 2.678494666091051801, 3.072372537026353267, -0.03421028094653036367 ) ) ;
#4737 = LINE ( 'NONE', #2741, #5038 ) ;
#4738 = VECTOR ( 'NONE', #3975, 1000.000000000000227 ) ;
#4739 = DIRECTION ( 'NONE',  ( -1.720845688168991849E-15, 1.000000000000000000, 6.656013887802284481E-31 ) ) ;
#4740 = CARTESIAN_POINT ( 'NONE',  ( 8.129778652391200566, -1.578738987863736565, 7.405931224841482141 ) ) ;
#4741 = PLANE ( 'NONE',  #15173 ) ;
#4742 = CARTESIAN_POINT ( 'NONE',  ( 1.387778780781445676E-14, 4.618802153517020059, 0.000000000000000000 ) ) ;
#4743 = ADVANCED_FACE ( 'NONE', ( #3279 ), #6927, .T. ) ;
#4744 = DIRECTION ( 'NONE',  ( -2.220446049250313081E-16, 1.000000000000000000, -7.025792437124636392E-31 ) ) ;
#4745 = DIRECTION ( 'NONE',  ( -1.000000000000000000, -3.254448077276381206E-32, -1.066788928082016908E-26 ) ) ;
#4746 = CARTESIAN_POINT ( 'NONE',  ( -43.10883117545714782, -4.565685424949276872, 7.500000000000062172 ) ) ;
#4747 = CARTESIAN_POINT ( 'NONE',  ( 3.878104551856317972, -0.7018542299754928493, -3.500000000000006661 ) ) ;
#4748 = EDGE_LOOP ( 'NONE', ( #5282, #13496, #12472, #6941 ) ) ;
#4749 = ADVANCED_FACE ( 'NONE', ( #14215 ), #10352, .T. ) ;
#4751 = ORIENTED_EDGE ( 'NONE', *, *, #4707, .F. ) ;
#4750 = EDGE_LOOP ( 'NONE', ( #23267, #3208, #14511, #14160 ) ) ;
#4752 = ORIENTED_EDGE ( 'NONE', *, *, #5353, .F. ) ;
#4753 = EDGE_CURVE ( 'NONE', #5440, #19516, #3969, .T. ) ;
#4754 = ORIENTED_EDGE ( 'NONE', *, *, #5134, .T. ) ;
#4755 = VERTEX_POINT ( 'NONE', #11764 ) ;
#4756 = ADVANCED_FACE ( 'NONE', ( #22594 ), #7044, .F. ) ;
#4757 = AXIS2_PLACEMENT_3D ( 'NONE', #15594, #6557, #13726 ) ;
#4758 = EDGE_LOOP ( 'NONE', ( #14700, #2295 ) ) ;
#4759 = LINE ( 'NONE', #16980, #19697 ) ;
#4760 = LINE ( 'NONE', #6071, #20798 ) ;
#4761 = VERTEX_POINT ( 'NONE', #4472 ) ;
#4762 = CARTESIAN_POINT ( 'NONE',  ( 57.15235153779114796, -1.074585193523325266, -6.499999999999977796 ) ) ;
#4763 = CARTESIAN_POINT ( 'NONE',  ( 3.511755186886688307, -2.826662030176431362, -3.597382984111577642 ) ) ;
#4764 = CARTESIAN_POINT ( 'NONE',  ( 4.170895651974849905, 2.054890354522574292, 3.559174498016395294 ) ) ;
#4765 = CARTESIAN_POINT ( 'NONE',  ( 42.50000000000014921, 0.4999999999999865663, -0.4999999999999726885 ) ) ;
#4766 = CARTESIAN_POINT ( 'NONE',  ( 108.2426266706970353, -6.527605602963587828, 6.500000000000199840 ) ) ;
#4767 = EDGE_CURVE ( 'NONE', #16772, #2264, #2461, .T. ) ;
#4768 = FILL_AREA_STYLE ('',( #20902 ) ) ;
#4769 = ADVANCED_FACE ( 'NONE', ( #21277 ), #9775, .F. ) ;
#4770 = FACE_OUTER_BOUND ( 'NONE', #10832, .T. ) ;
#4771 = CARTESIAN_POINT ( 'NONE',  ( 5.100000000000000533, 0.000000000000000000, -3.469446951953614189E-15 ) ) ;
#4772 = FACE_OUTER_BOUND ( 'NONE', #18415, .T. ) ;
#4773 = CIRCLE ( 'NONE', #20940, 4.500000000000045297 ) ;
#4774 = ORIENTED_EDGE ( 'NONE', *, *, #2601, .F. ) ;
#4775 = ADVANCED_FACE ( 'NONE', ( #8802 ), #15957, .T. ) ;
#4776 = COLOUR_RGB ( '', 0.09019608, 0.27058824, 0.51372549) ;
#4777 = CARTESIAN_POINT ( 'NONE',  ( 0.000000000000000000, 0.000000000000000000, 0.000000000000000000 ) ) ;
#4778 = DIRECTION ( 'NONE',  ( 0.000000000000000000, -3.382522293539642681E-32, -1.000000000000000000 ) ) ;
#4779 = ORIENTED_EDGE ( 'NONE', *, *, #1648, .T. ) ;
#4780 = TOROIDAL_SURFACE ( 'NONE', #17942, 4.500000000000000888, 0.5000000000000000000 ) ;
#4781 = ADVANCED_FACE ( 'NONE', ( #7381 ), #11107, .T. ) ;
#4782 = ORIENTED_EDGE ( 'NONE', *, *, #10486, .T. ) ;
#4783 = VERTEX_POINT ( 'NONE', #5737 ) ;
#4784 = EDGE_CURVE ( 'NONE', #13378, #18638, #17108, .T. ) ;
#4785 = ORIENTED_EDGE ( 'NONE', *, *, #7109, .F. ) ;
#4786 = CARTESIAN_POINT ( 'NONE',  ( -50.65685424949275983, 7.200000000000018829, -8.000000000000007105 ) ) ;
#4787 = DIRECTION ( 'NONE',  ( 2.478176394252584494E-15, -7.888609052210165348E-31, 1.000000000000000000 ) ) ;
#4788 = ORIENTED_EDGE ( 'NONE', *, *, #12520, .T. ) ;
#4789 = AXIS2_PLACEMENT_3D ( 'NONE', #11624, #16556, #466 ) ;
#4790 = CARTESIAN_POINT ( 'NONE',  ( 24.75000000000001776, 1.250000000000001110, -17.00000000000001066 ) ) ;
#4791 = DIRECTION ( 'NONE',  ( 3.885780586188016830E-16, 4.437342591868156373E-31, -1.000000000000000000 ) ) ;
#4792 = VECTOR ( 'NONE', #12564, 1000.000000000000000 ) ;
#4793 = DIRECTION ( 'NONE',  ( -1.000000000000000000, 0.000000000000000000, -2.668805347656595124E-16 ) ) ;
#4794 = DIRECTION ( 'NONE',  ( -1.000000000000000000, 1.399221158233660042E-15, 0.000000000000000000 ) ) ;
#4795 = CARTESIAN_POINT ( 'NONE',  ( 3.878096787214385444, 3.381939201670001616, 1.142309474598473873 ) ) ;
#4796 = CIRCLE ( 'NONE', #11176, 2.499999999999990674 ) ;
#4797 = CARTESIAN_POINT ( 'NONE',  ( -7.651206356577011647, -0.8338323182647964238, 8.300907142094176905 ) ) ;
#4798 = EDGE_CURVE ( 'NONE', #1665, #14963, #13002, .T. ) ;
#4799 = CONICAL_SURFACE ( 'NONE', #681, 4.000000000000022204, 0.8911886515913840512 ) ;
#4800 = DIRECTION ( 'NONE',  ( -7.395570986446975166E-31, -3.382522293539642681E-32, -1.000000000000000000 ) ) ;
#4801 = AXIS2_PLACEMENT_3D ( 'NONE', #20267, #11199, #18836 ) ;
#4802 = EDGE_CURVE ( 'NONE', #9470, #7130, #12783, .T. ) ;
#4803 = DIRECTION ( 'NONE',  ( 0.000000000000000000, 0.000000000000000000, -1.000000000000000000 ) ) ;
#4804 = DIRECTION ( 'NONE',  ( -2.013525853228507892E-32, -6.902532920683810383E-31, 1.000000000000000000 ) ) ;
#4805 = CARTESIAN_POINT ( 'NONE',  ( -10.49999999999998224, -12.00000000000002842, 5.750000000000018652 ) ) ;
#4807 = AXIS2_PLACEMENT_3D ( 'NONE', #18754, #19099, #13576 ) ;
#4806 = DIRECTION ( 'NONE',  ( 2.013525853228507892E-32, 6.902532920683810383E-31, -1.000000000000000000 ) ) ;
#4808 = CARTESIAN_POINT ( 'NONE',  ( 2.500000000000000444, 0.000000000000000000, 3.415236843329338967E-15 ) ) ;
#4809 = ORIENTED_EDGE ( 'NONE', *, *, #19052, .F. ) ;
#4810 = ADVANCED_FACE ( 'NONE', ( #1732 ), #8482, .T. ) ;
#4811 = ORIENTED_EDGE ( 'NONE', *, *, #2623, .T. ) ;
#4812 = CIRCLE ( 'NONE', #17975, 0.2500000000000002220 ) ;
#4813 = VECTOR ( 'NONE', #17382, 1000.000000000000000 ) ;
#4815 = ORIENTED_EDGE ( 'NONE', *, *, #13276, .F. ) ;
#4814 = ORIENTED_EDGE ( 'NONE', *, *, #7145, .F. ) ;
#4816 = AXIS2_PLACEMENT_3D ( 'NONE', #23, #21547, #15990 ) ;
#4817 = CARTESIAN_POINT ( 'NONE',  ( 7.500000000000007105, -8.000000000000010658, 10.75000000000000888 ) ) ;
#4818 = CARTESIAN_POINT ( 'NONE',  ( -89.70000000000064233, 5.551115123125782702E-14, -2.000000000000001776 ) ) ;
#4819 = FACE_OUTER_BOUND ( 'NONE', #18298, .T. ) ;
#4820 = ORIENTED_EDGE ( 'NONE', *, *, #3646, .F. ) ;
#4821 = DIRECTION ( 'NONE',  ( 2.013525853228507892E-32, 6.902532920683810383E-31, -1.000000000000000000 ) ) ;
#4822 = DIRECTION ( 'NONE',  ( -0.7071067811865490160, -0.7071067811865460184, -1.565905175853766674E-16 ) ) ;
#4823 = CARTESIAN_POINT ( 'NONE',  ( 0.000000000000000000, 0.000000000000000000, 0.000000000000000000 ) ) ;
#4824 = PLANE ( 'NONE',  #6878 ) ;
#4825 = DIRECTION ( 'NONE',  ( 8.438582421954110511E-32, 0.000000000000000000, 1.000000000000000000 ) ) ;
#4826 = CARTESIAN_POINT ( 'NONE',  ( -6.000000000000130562, 7.999999999999958256, -8.000000000000035527 ) ) ;
#4827 = CARTESIAN_POINT ( 'NONE',  ( -67.40537636629493079, 0.5000000000000143219, 12.70639812373644517 ) ) ;
#4828 = DIRECTION ( 'NONE',  ( -2.220446049250313081E-16, 1.000000000000000000, -7.025792437124636392E-31 ) ) ;
#4829 = EDGE_CURVE ( 'NONE', #17901, #13088, #5482, .T. ) ;
#4830 = AXIS2_PLACEMENT_3D ( 'NONE', #1293, #8231, #4913 ) ;
#4831 = AXIS2_PLACEMENT_3D ( 'NONE', #13025, #2308, #11019 ) ;
#4832 = DIRECTION ( 'NONE',  ( -1.000000000000000000, 4.190823558986610327E-31, -1.733449886265890494E-32 ) ) ;
#4833 = AXIS2_PLACEMENT_3D ( 'NONE', #14063, #21484, #16044 ) ;
#4834 = CARTESIAN_POINT ( 'NONE',  ( 4.124214193018073793, -4.056676826581885997, 3.830195444513743874E-18 ) ) ;
#4835 = EDGE_LOOP ( 'NONE', ( #21035, #15370, #2143, #8716 ) ) ;
#4836 = CARTESIAN_POINT ( 'NONE',  ( -57.51225780766257856, -8.340516433293975851, 19.16570243528392936 ) ) ;
#4838 = ORIENTED_EDGE ( 'NONE', *, *, #5054, .T. ) ;
#4837 = ORIENTED_EDGE ( 'NONE', *, *, #204, .F. ) ;
#4839 = UNCERTAINTY_MEASURE_WITH_UNIT (LENGTH_MEASURE( 1.000000000000000082E-05 ), #16167, 'distance_accuracy_value', 'NONE');
#4840 = ADVANCED_FACE ( 'NONE', ( #21515 ), #7496, .T. ) ;
#4841 = ORIENTED_EDGE ( 'NONE', *, *, #21449, .T. ) ;
#4843 = EDGE_LOOP ( 'NONE', ( #11634, #12390, #14016, #4525 ) ) ;
#4842 = ORIENTED_EDGE ( 'NONE', *, *, #8094, .F. ) ;
#4844 = DIRECTION ( 'NONE',  ( -1.000000000000000000, 0.000000000000000000, -3.717264591378832268E-16 ) ) ;
#4845 = CARTESIAN_POINT ( 'NONE',  ( -4.203833317240987633, -1.627343821129589418, -3.597273115243885044 ) ) ;
#4846 = LINE ( 'NONE', #15658, #8722 ) ;
#4847 = CIRCLE ( 'NONE', #12742, 2.999999999999995559 ) ;
#4848 = CARTESIAN_POINT ( 'NONE',  ( 5.560781378645605066, -6.418764338089353846E-15, -3.999999999999992450 ) ) ;
#4849 = DIRECTION ( 'NONE',  ( 2.013525853228507892E-32, 6.902532920683810383E-31, -1.000000000000000000 ) ) ;
#4850 = CARTESIAN_POINT ( 'NONE',  ( -6.938893903907228378E-14, 0.7368602791855416445, -1.387778780781445676E-14 ) ) ;
#4851 = CARTESIAN_POINT ( 'NONE',  ( -6.000000000000102141, 5.299999999999964295, 8.000000000000047962 ) ) ;
#4852 = DIRECTION ( 'NONE',  ( 1.000000000000000000, -1.276756478318922922E-15, 1.342094922251465017E-15 ) ) ;
#4853 = COLOUR_RGB ( '', 0.72549020, 0.75294118, 0.79215686) ;
#4854 = CARTESIAN_POINT ( 'NONE',  ( 4.030875481282551576, 1.403567514398184723, 3.499999999999968026 ) ) ;
#4855 =( NAMED_UNIT ( * ) SI_UNIT ( $, .STERADIAN. ) SOLID_ANGLE_UNIT ( ) );
#4856 = DIRECTION ( 'NONE',  ( -1.000000000000000000, 0.000000000000000000, -1.066742637285843118E-26 ) ) ;
#4857 = DIRECTION ( 'NONE',  ( 0.000000000000000000, 0.000000000000000000, 1.000000000000000000 ) ) ;
#4858 = FACE_OUTER_BOUND ( 'NONE', #2665, .T. ) ;
#4859 = CARTESIAN_POINT ( 'NONE',  ( 4.052424581287934480, -2.393186648133822203, 2.990837702970649215 ) ) ;
#4860 = ORIENTED_EDGE ( 'NONE', *, *, #11239, .T. ) ;
#4862 = VERTEX_POINT ( 'NONE', #436 ) ;
#4861 = ORIENTED_EDGE ( 'NONE', *, *, #11822, .T. ) ;
#4863 = VERTEX_POINT ( 'NONE', #14664 ) ;
#4864 = ORIENTED_EDGE ( 'NONE', *, *, #12932, .F. ) ;
#4865 = AXIS2_PLACEMENT_3D ( 'NONE', #3366, #17693, #6887 ) ;
#4866 = ORIENTED_EDGE ( 'NONE', *, *, #22624, .F. ) ;
#4867 = STYLED_ITEM ( 'NONE', ( #9786 ), #2433 ) ;
#4868 = ORIENTED_EDGE ( 'NONE', *, *, #17260, .F. ) ;
#4869 = FACE_OUTER_BOUND ( 'NONE', #8868, .T. ) ;
#4870 = CARTESIAN_POINT ( 'NONE',  ( -7.499999999999992895, -8.000000000000044409, 6.250000000000005329 ) ) ;
#4871 = VERTEX_POINT ( 'NONE', #3725 ) ;
#4872 = DIRECTION ( 'NONE',  ( 0.000000000000000000, 0.000000000000000000, 1.000000000000000000 ) ) ;
#4873 = CARTESIAN_POINT ( 'NONE',  ( 2.339468227445713921, 3.268109542640643905, -5.600000000000002309 ) ) ;
#4874 = EDGE_CURVE ( 'NONE', #5583, #18644, #3957, .T. ) ;
#4875 = LINE ( 'NONE', #8647, #14380 ) ;
#4876 = CARTESIAN_POINT ( 'NONE',  ( 30.15500000000000114, 2.775557561562891351E-14, -2.081668171172168513E-14 ) ) ;
#4877 = B_SPLINE_CURVE_WITH_KNOTS ( 'NONE', 3,
 ( #528, #16498, #14636, #14744, #22045, #5706 ),
 .UNSPECIFIED., .F., .F.,
 ( 4, 2, 4 ),
 ( 0.002452478801916372839, 0.003676905084148008283, 0.004901331366379643728 ),
 .UNSPECIFIED. ) ;
#4878 = PLANE ( 'NONE',  #5712 ) ;
#4879 = PLANE ( 'NONE',  #9626 ) ;
#4880 = CARTESIAN_POINT ( 'NONE',  ( -3.122502256758252770E-14, 59.74999999999991473, 2.081668171172168513E-14 ) ) ;
#4881 = CARTESIAN_POINT ( 'NONE',  ( 2.000000000000015543, -3.464101615137746837, 0.000000000000000000 ) ) ;
#4882 = AXIS2_PLACEMENT_3D ( 'NONE', #14493, #7664, #21678 ) ;
#4883 = LINE ( 'NONE', #9010, #11784 ) ;
#4884 =( REPRESENTATION_RELATIONSHIP ('NONE','NONE', #19450, #17033 ) REPRESENTATION_RELATIONSHIP_WITH_TRANSFORMATION ( #7759 )SHAPE_REPRESENTATION_RELATIONSHIP( ) );
#4885 = CARTESIAN_POINT ( 'NONE',  ( 42.50000000000014921, 8.000000000000003553, -0.4999999999999726885 ) ) ;
#4886 = CARTESIAN_POINT ( 'NONE',  ( -6.000000000000143885, -2.000000000000043521, -8.000000000000035527 ) ) ;
#4887 = VERTEX_POINT ( 'NONE', #10895 ) ;
#4888 = CARTESIAN_POINT ( 'NONE',  ( 3.948103430091018939, 3.379418997638859778, 1.146674596026393100 ) ) ;
#4889 = CARTESIAN_POINT ( 'NONE',  ( 2.869123094150540578E-16, -6.219541108242227082E-16, -4.750000000000000000 ) ) ;
#4891 = ORIENTED_EDGE ( 'NONE', *, *, #14528, .T. ) ;
#4890 = ORIENTED_EDGE ( 'NONE', *, *, #2050, .T. ) ;
#4892 = ORIENTED_EDGE ( 'NONE', *, *, #14586, .F. ) ;
#4893 = DIRECTION ( 'NONE',  ( -2.013525853228507892E-32, -6.902532920683810383E-31, 1.000000000000000000 ) ) ;
#4894 = EDGE_CURVE ( 'NONE', #10831, #7035, #12625, .T. ) ;
#4895 = CARTESIAN_POINT ( 'NONE',  ( 2.918498775983380256E-10, 2.999999999003851503, -32.00000000000000000 ) ) ;
#4896 = ORIENTED_EDGE ( 'NONE', *, *, #16010, .T. ) ;
#4897 = VECTOR ( 'NONE', #11641, 1000.000000000000000 ) ;
#4898 = CARTESIAN_POINT ( 'NONE',  ( -42.54314575050785407, -8.000000000000000000, -7.500000000000007105 ) ) ;
#4899 = CARTESIAN_POINT ( 'NONE',  ( 58.04599508018838350, 2.194061104857397915, -5.999999999999991118 ) ) ;
#4900 = FACE_OUTER_BOUND ( 'NONE', #9767, .T. ) ;
#4901 = EDGE_CURVE ( 'NONE', #10858, #11150, #7606, .T. ) ;
#4902 = CARTESIAN_POINT ( 'NONE',  ( -6.566827241915921043, 35.99999999896398606, -18.68676989095779462 ) ) ;
#4903 = PLANE ( 'NONE',  #16070 ) ;
#4904 = DIRECTION ( 'NONE',  ( 1.066786462891689527E-26, 6.656013887802287108E-31, 1.000000000000000000 ) ) ;
#4905 = FACE_OUTER_BOUND ( 'NONE', #8751, .T. ) ;
#4906 = CARTESIAN_POINT ( 'NONE',  ( 0.000000000000000000, 10.49999999999999822, -10.86602540378443749 ) ) ;
#4907 = EDGE_CURVE ( 'NONE', #12159, #20325, #3617, .T. ) ;
#4908 = ADVANCED_FACE ( 'NONE', ( #14784, #1952, #3620 ), #3835, .F. ) ;
#4909 = FACE_BOUND ( 'NONE', #4117, .T. ) ;
#4910 = CARTESIAN_POINT ( 'NONE',  ( 73.50000000000115108, -6.999999999999811706, -6.938893903907228378E-15 ) ) ;
#4912 = ADVANCED_FACE ( 'NONE', ( #5858 ), #15627, .T. ) ;
#4911 = DIRECTION ( 'NONE',  ( -1.000000000000000000, -0.000000000000000000, 0.000000000000000000 ) ) ;
#4913 = DIRECTION ( 'NONE',  ( -1.000000000000000000, 0.000000000000000000, 0.000000000000000000 ) ) ;
#4914 = AXIS2_PLACEMENT_3D ( 'NONE', #22369, #11296, #6251 ) ;
#4915 = VECTOR ( 'NONE', #326, 1000.000000000000000 ) ;
#4916 = VERTEX_POINT ( 'NONE', #17858 ) ;
#4917 = ORIENTED_EDGE ( 'NONE', *, *, #13149, .T. ) ;
#4918 = ADVANCED_FACE ( 'NONE', ( #6400 ), #18210, .T. ) ;
#4919 = CARTESIAN_POINT ( 'NONE',  ( -4.550510256924973795, 35.99999999900384751, -25.99999999999999645 ) ) ;
#4920 = EDGE_CURVE ( 'NONE', #8376, #22529, #17505, .T. ) ;
#4921 = EDGE_CURVE ( 'NONE', #21322, #11731, #3991, .T. ) ;
#4923 = ORIENTED_EDGE ( 'NONE', *, *, #16684, .F. ) ;
#4922 = ORIENTED_EDGE ( 'NONE', *, *, #23030, .F. ) ;
#4924 = VERTEX_POINT ( 'NONE', #9961 ) ;
#4925 = DIRECTION ( 'NONE',  ( -4.190823558986625216E-31, 1.000000000000000000, -4.190823558986625216E-31 ) ) ;
#4926 = VERTEX_POINT ( 'NONE', #18656 ) ;
#4927 = FACE_OUTER_BOUND ( 'NONE', #20163, .T. ) ;
#4928 = CARTESIAN_POINT ( 'NONE',  ( -5.549486778973212076, 36.19267127072036772, -26.13446119014969327 ) ) ;
#4929 = VERTEX_POINT ( 'NONE', #2659 ) ;
#4930 = DIRECTION ( 'NONE',  ( 1.000000000000000000, 0.000000000000000000, 0.000000000000000000 ) ) ;
#4931 = CIRCLE ( 'NONE', #21086, 5.999999999999998224 ) ;
#4932 = CIRCLE ( 'NONE', #17716, 5.560781378645605066 ) ;
#4933 = DIRECTION ( 'NONE',  ( 1.000000000000000000, 2.699383410053119644E-30, 3.330669073875432643E-16 ) ) ;
#4934 = ADVANCED_FACE ( 'NONE', ( #9727 ), #20635, .T. ) ;
#4935 = PLANE ( 'NONE',  #1276 ) ;
#4936 = DIRECTION ( 'NONE',  ( 2.013525853228507892E-32, 6.902532920683810383E-31, -1.000000000000000000 ) ) ;
#4937 = EDGE_CURVE ( 'NONE', #17297, #9451, #15041, .T. ) ;
#4938 = DIRECTION ( 'NONE',  ( -4.019602852144232182E-47, -6.982962677686261977E-15, -1.000000000000000000 ) ) ;
#4939 = DIRECTION ( 'NONE',  ( -1.577021341797097314E-16, 1.000000000000000000, -3.627149086133324068E-15 ) ) ;
#4941 = EDGE_CURVE ( 'NONE', #23235, #172, #18143, .T. ) ;
#4940 = CARTESIAN_POINT ( 'NONE',  ( 61.48996577904082272, -5.119475911334187224, -5.999999999999928946 ) ) ;
#4942 = LINE ( 'NONE', #12111, #9324 ) ;
#4943 = CARTESIAN_POINT ( 'NONE',  ( 0.000000000000000000, 0.000000000000000000, 0.000000000000000000 ) ) ;
#4944 = VERTEX_POINT ( 'NONE', #8538 ) ;
#4945 = DIRECTION ( 'NONE',  ( 1.000000000000000000, 0.000000000000000000, 0.000000000000000000 ) ) ;
#4946 = VECTOR ( 'NONE', #11352, 1000.000000000000000 ) ;
#4947 = CIRCLE ( 'NONE', #5726, 3.500000000000023981 ) ;
#4949 = ORIENTED_EDGE ( 'NONE', *, *, #6064, .T. ) ;
#4948 = ORIENTED_EDGE ( 'NONE', *, *, #17273, .T. ) ;
#4950 = ORIENTED_EDGE ( 'NONE', *, *, #9950, .F. ) ;
#4952 = ORIENTED_EDGE ( 'NONE', *, *, #6231, .F. ) ;
#4951 = ORIENTED_EDGE ( 'NONE', *, *, #15535, .T. ) ;
#4953 = ORIENTED_EDGE ( 'NONE', *, *, #17828, .T. ) ;
#4954 = CARTESIAN_POINT ( 'NONE',  ( -42.54314575050793934, -8.000000000000021316, 7.500000000000062172 ) ) ;
#4955 = CARTESIAN_POINT ( 'NONE',  ( -50.65685424949273141, 7.200000000000025935, 8.000000000000076383 ) ) ;
#4956 = DIRECTION ( 'NONE',  ( 0.000000000000000000, 0.000000000000000000, 1.000000000000000000 ) ) ;
#4957 = CARTESIAN_POINT ( 'NONE',  ( 1.500000000000004885, 3.812371101874739144E-16, -3.113037248396080425 ) ) ;
#4958 =( GEOMETRIC_REPRESENTATION_CONTEXT ( 3 ) GLOBAL_UNCERTAINTY_ASSIGNED_CONTEXT ( ( #16374 ) ) GLOBAL_UNIT_ASSIGNED_CONTEXT ( ( #6176, #876, #4855 ) ) REPRESENTATION_CONTEXT ( 'NONE', 'WORKASPACE' ) );
#4959 = DIRECTION ( 'NONE',  ( -0.000000000000000000, -0.000000000000000000, 1.000000000000000000 ) ) ;
#4960 = ADVANCED_FACE ( 'NONE', ( #19016, #22778, #8651 ), #4879, .F. ) ;
#4961 = CARTESIAN_POINT ( 'NONE',  ( 54.42435809754109499, 0.000000000000000000, 6.500000000000144773 ) ) ;
#4962 = LINE ( 'NONE', #18982, #3839 ) ;
#4963 = DIRECTION ( 'NONE',  ( 1.000000000000000000, -4.615739097524200579E-16, -1.134196829589820086E-15 ) ) ;
#4964 = CARTESIAN_POINT ( 'NONE',  ( 0.3263565795980740147, -4.430380094434307026, -0.2484800633750381682 ) ) ;
#4965 = AXIS2_PLACEMENT_3D ( 'NONE', #3470, #10980, #5475 ) ;
#4966 = CARTESIAN_POINT ( 'NONE',  ( 3.880214671983731822, -0.7309020039786242595, 3.499999999999996003 ) ) ;
#4967 = AXIS2_PLACEMENT_3D ( 'NONE', #19036, #13272, #8326 ) ;
#4968 = DIRECTION ( 'NONE',  ( 0.000000000000000000, -1.387778780781440785E-14, 1.000000000000000000 ) ) ;
#4969 = AXIS2_PLACEMENT_3D ( 'NONE', #5855, #16642, #22074 ) ;
#4970 = EDGE_CURVE ( 'NONE', #19164, #18123, #15252, .T. ) ;
#4971 = CIRCLE ( 'NONE', #20780, 2.549999999999997158 ) ;
#4972 = CARTESIAN_POINT ( 'NONE',  ( 37.00000000000014211, 0.000000000000000000, -3.000000000000002665 ) ) ;
#4973 = DIRECTION ( 'NONE',  ( 0.000000000000000000, 0.000000000000000000, -1.000000000000000000 ) ) ;
#4974 = DIRECTION ( 'NONE',  ( -1.000000000000000000, -2.172745813409349776E-17, 2.775557561562883647E-17 ) ) ;
#4975 = CARTESIAN_POINT ( 'NONE',  ( 1.462430223138485341E-14, -22.49999999999995381, -7.882182279042456940 ) ) ;
#4976 = PRODUCT ( 'Rubber Head', 'Rubber Head', '', ( #10712 ) ) ;
#4977 = ORIENTED_EDGE ( 'NONE', *, *, #12114, .T. ) ;
#4978 = AXIS2_PLACEMENT_3D ( 'NONE', #3679, #4235, #7777 ) ;
#4980 = ORIENTED_EDGE ( 'NONE', *, *, #20945, .T. ) ;
#4979 = ORIENTED_EDGE ( 'NONE', *, *, #21482, .F. ) ;
#4981 = EDGE_CURVE ( 'NONE', #22384, #11457, #12507, .T. ) ;
#4982 = ORIENTED_EDGE ( 'NONE', *, *, #21771, .F. ) ;
#4983 = ORIENTED_EDGE ( 'NONE', *, *, #10486, .F. ) ;
#4984 = CIRCLE ( 'NONE', #4217, 2.549999999999998934 ) ;
#4985 = ORIENTED_EDGE ( 'NONE', *, *, #3933, .F. ) ;
#4986 = CIRCLE ( 'NONE', #12887, 0.5000000000000006661 ) ;
#4987 = VECTOR ( 'NONE', #8305, 1000.000000000000000 ) ;
#4988 = VECTOR ( 'NONE', #19084, 1000.000000000000000 ) ;
#4989 = ORIENTED_EDGE ( 'NONE', *, *, #1153, .F. ) ;
#4990 = DIRECTION ( 'NONE',  ( 1.000000000000000000, -4.440892098500650814E-16, -7.860214984771113767E-18 ) ) ;
#4991 = DIRECTION ( 'NONE',  ( -1.000000000000000000, 0.000000000000000000, 0.000000000000000000 ) ) ;
#4992 = EDGE_LOOP ( 'NONE', ( #2465, #21053, #12686, #11509 ) ) ;
#4993 = PLANE ( 'NONE',  #1860 ) ;
#4994 = CARTESIAN_POINT ( 'NONE',  ( 3.973110223765529803, 0.6902454861566474920, -3.565797985667399139 ) ) ;
#4995 = DIRECTION ( 'NONE',  ( 1.000000000000000000, -1.365024226554777580E-62, 2.013525853228508439E-32 ) ) ;
#4996 = CARTESIAN_POINT ( 'NONE',  ( 0.000000000000000000, 0.000000000000000000, 0.000000000000000000 ) ) ;
#4997 = FACE_OUTER_BOUND ( 'NONE', #20249, .T. ) ;
#4998 = DIRECTION ( 'NONE',  ( 1.000000000000000000, 0.000000000000000000, 0.000000000000000000 ) ) ;
#4999 = DIRECTION ( 'NONE',  ( -1.000000000000000000, -1.479114197289397135E-31, -5.916456789157588541E-31 ) ) ;
#5000 = CARTESIAN_POINT ( 'NONE',  ( 37.86602540378461157, 11.00000000000000000, -10.86602540378450676 ) ) ;
#5001 = AXIS2_PLACEMENT_3D ( 'NONE', #8248, #13539, #10011 ) ;
#5002 = CARTESIAN_POINT ( 'NONE',  ( -6.999999999708143683, 13.99999999900385106, -18.79789498886801624 ) ) ;
#5003 = AXIS2_PLACEMENT_3D ( 'NONE', #9407, #19986, #15030 ) ;
#5004 = CARTESIAN_POINT ( 'NONE',  ( -6.495190528383328221, -4.163336342344337027E-14, 3.750000000000038192 ) ) ;
#5005 = AXIS2_PLACEMENT_3D ( 'NONE', #7440, #5681, #20021 ) ;
#5006 = ORIENTED_EDGE ( 'NONE', *, *, #8339, .T. ) ;
#5007 = AXIS2_PLACEMENT_3D ( 'NONE', #20281, #6162, #2150 ) ;
#5008 = SURFACE_STYLE_FILL_AREA ( #8782 ) ;
#5009 = DIRECTION ( 'NONE',  ( -0.7071067811865474617, 0.7071067811865474617, -0.000000000000000000 ) ) ;
#5010 = CARTESIAN_POINT ( 'NONE',  ( 4.211140560182194292, -2.431303136016568889, -3.745885042887441063 ) ) ;
#5012 = ORIENTED_EDGE ( 'NONE', *, *, #9614, .F. ) ;
#5011 = ORIENTED_EDGE ( 'NONE', *, *, #16231, .T. ) ;
#5013 = ADVANCED_FACE ( 'NONE', ( #6893 ), #14067, .F. ) ;
#5014 = ORIENTED_EDGE ( 'NONE', *, *, #10214, .T. ) ;
#5015 = EDGE_CURVE ( 'NONE', #11319, #17475, #3374, .T. ) ;
#5016 = VERTEX_POINT ( 'NONE', #15589 ) ;
#5017 = CARTESIAN_POINT ( 'NONE',  ( 4.104070371397483541, 2.023683613428369110, 3.505122836902505146 ) ) ;
#5018 = FACE_OUTER_BOUND ( 'NONE', #12799, .T. ) ;
#5019 = VECTOR ( 'NONE', #14899, 1000.000000000000000 ) ;
#5020 =( BOUNDED_SURFACE ( )  B_SPLINE_SURFACE ( 3, 2, ( 
 ( #14261, #14368, #255 ),
 ( #9309, #21675, #20128 ),
 ( #5555, #20013, #19670 ),
 ( #12954, #10721, #3560 ),
 ( #17908, #4002, #12721 ),
 ( #12602, #19906, #39 ),
 ( #7432, #19787, #21450 ),
 ( #21790, #2246, #3772 ),
 ( #1888, #18250, #2121 ),
 ( #14706, #14603, #3666 ),
 ( #10838, #21896, #9073 ),
 ( #10941, #16572, #2007 ),
 ( #16232, #150, #18369 ),
 ( #9196, #22366, #9541 ) ),
 .UNSPECIFIED., .F., .F., .T. ) 
 B_SPLINE_SURFACE_WITH_KNOTS ( ( 4, 2, 2, 2, 2, 2, 4 ),
 ( 3, 3 ),
 ( 0.000000000000000000, 0.0009656398008937971521, 0.001448459701340695620, 0.001931279601787594304, 0.002414099502234492989, 0.002896919402681391240, 0.003862559203575188609 ),
 ( 0.000000000000000000, 1.000000000000000000 ),
 .UNSPECIFIED. ) 
 GEOMETRIC_REPRESENTATION_ITEM ( )  RATIONAL_B_SPLINE_SURFACE ( (
 ( 1.000000000000000000, 0.7071067811865429098, 1.000000000000000000),
 ( 1.000000000000000000, 0.6907538105667043737, 1.000000000000000000),
 ( 1.000000000000000000, 0.6765417438350033175, 1.000000000000000000),
 ( 1.000000000000000000, 0.6623232117678236053, 1.000000000000000000),
 ( 1.000000000000000000, 0.6588386061805659999, 1.000000000000000000),
 ( 1.000000000000000000, 0.6547992448372328411, 1.000000000000000000),
 ( 1.000000000000000000, 0.6542040191408873273, 1.000000000000000000),
 ( 1.000000000000000000, 0.6557724471762160778, 1.000000000000000000),
 ( 1.000000000000000000, 0.6579729115737033007, 1.000000000000000000),
 ( 1.000000000000000000, 0.6644691908065228914, 1.000000000000000000),
 ( 1.000000000000000000, 0.6687559023949211090, 1.000000000000000000),
 ( 1.000000000000000000, 0.6835702420294266224, 1.000000000000000000),
 ( 1.000000000000000000, 0.6960226107070131008, 1.000000000000000000),
 ( 1.000000000000000000, 0.7071067811865431318, 1.000000000000000000) ) ) 
 REPRESENTATION_ITEM ( '' )  SURFACE ( )  );
#5021 = CIRCLE ( 'NONE', #15163, 7.000000000000000000 ) ;
#5022 = CARTESIAN_POINT ( 'NONE',  ( 7.523653856849480626, -1.079621694564734780, 8.801128846369474346 ) ) ;
#5023 = VECTOR ( 'NONE', #20822, 1000.000000000000000 ) ;
#5024 = TOROIDAL_SURFACE ( 'NONE', #11399, 4.500000000000000888, 0.5000000000000000000 ) ;
#5025 = CARTESIAN_POINT ( 'NONE',  ( -5.036205380386646446, 1.584759246591022297, 0.7770364038185694211 ) ) ;
#5026 = DIRECTION ( 'NONE',  ( -1.000000000000000000, 4.615739097524200579E-16, 1.134196829589820086E-15 ) ) ;
#5027 = AXIS2_PLACEMENT_3D ( 'NONE', #1075, #13651, #19057 ) ;
#5028 = CARTESIAN_POINT ( 'NONE',  ( -6.892555770682806857E-14, 0.7368602791855416445, 4.749999999999985789 ) ) ;
#5029 = LINE ( 'NONE', #3501, #13471 ) ;
#5030 =( REPRESENTATION_RELATIONSHIP ('NONE','NONE', #19450, #10586 ) REPRESENTATION_RELATIONSHIP_WITH_TRANSFORMATION ( #19778 )SHAPE_REPRESENTATION_RELATIONSHIP( ) );
#5031 = CARTESIAN_POINT ( 'NONE',  ( -6.000000000000088818, -2.000000000000043521, 7.500000000000076383 ) ) ;
#5032 = CARTESIAN_POINT ( 'NONE',  ( 3.973514160553465402, -2.741076955031368279, -2.383932505289874548 ) ) ;
#5033 = CARTESIAN_POINT ( 'NONE',  ( 30.00000000029184832, -0.5000000009961480529, -5.999999999999998224 ) ) ;
#5034 = DIRECTION ( 'NONE',  ( 1.577021341797097314E-16, 1.000000000000000000, 0.000000000000000000 ) ) ;
#5035 = DIRECTION ( 'NONE',  ( -0.4999999999999999445, -2.286725509617068974E-17, 0.8660254037844387076 ) ) ;
#5036 = CARTESIAN_POINT ( 'NONE',  ( 42.00000000000014921, 0.5000000000000143219, 2.500000000000030198 ) ) ;
#5037 = LINE ( 'NONE', #3286, #7735 ) ;
#5038 = VECTOR ( 'NONE', #991, 1000.000000000000000 ) ;
#5039 = DIRECTION ( 'NONE',  ( 1.000000000000000000, 0.000000000000000000, 1.066788928082016908E-26 ) ) ;
#5040 = CIRCLE ( 'NONE', #16319, 6.500000000000075495 ) ;
#5041 = DIRECTION ( 'NONE',  ( 1.000000000000000000, 0.000000000000000000, 0.000000000000000000 ) ) ;
#5042 = VERTEX_POINT ( 'NONE', #21130 ) ;
#5043 = VECTOR ( 'NONE', #18396, 999.9999999999998863 ) ;
#5044 = EDGE_CURVE ( 'NONE', #7934, #10595, #8130, .T. ) ;
#5045 = ORIENTED_EDGE ( 'NONE', *, *, #21414, .T. ) ;
#5046 = VERTEX_POINT ( 'NONE', #6552 ) ;
#5047 = CARTESIAN_POINT ( 'NONE',  ( -5.273209981518101053, 36.26961333663654585, -26.07660499612833149 ) ) ;
#5050 = ORIENTED_EDGE ( 'NONE', *, *, #1487, .T. ) ;
#5049 = ADVANCED_FACE ( 'NONE', ( #17701 ), #13831, .T. ) ;
#5048 = ORIENTED_EDGE ( 'NONE', *, *, #7234, .T. ) ;
#5051 = ADVANCED_FACE ( 'NONE', ( #22662 ), #13642, .T. ) ;
#5052 = B_SPLINE_CURVE_WITH_KNOTS ( 'NONE', 3,
 ( #6623, #2985, #22629, #1448, #8622, #10156 ),
 .UNSPECIFIED., .F., .F.,
 ( 4, 2, 4 ),
 ( 0.002365888236228034115, 0.003551327329835107967, 0.004736766423442182253 ),
 .UNSPECIFIED. ) ;
#5053 = CARTESIAN_POINT ( 'NONE',  ( 1.257172072275264174, -3.892973519171180730, -3.433252694550784856 ) ) ;
#5054 = EDGE_CURVE ( 'NONE', #20178, #6969, #17771, .T. ) ;
#5055 = ORIENTED_EDGE ( 'NONE', *, *, #16336, .F. ) ;
#5056 = CARTESIAN_POINT ( 'NONE',  ( 73.50000000000116529, -6.999999999999811706, 2.549999999999985612 ) ) ;
#5057 = FILL_AREA_STYLE ('',( #6593 ) ) ;
#5058 = CARTESIAN_POINT ( 'NONE',  ( 61.83096495907212642, -4.753799060524616316, -6.500000000000012434 ) ) ;
#5059 = CIRCLE ( 'NONE', #13711, 6.500000000000075495 ) ;
#5060 = ORIENTED_EDGE ( 'NONE', *, *, #14675, .T. ) ;
#5061 = DIRECTION ( 'NONE',  ( -1.000000000000000000, 1.365024226554778012E-62, -2.013525853228508439E-32 ) ) ;
#5062 = CARTESIAN_POINT ( 'NONE',  ( 4.071447262713884463, 2.020725942163639655, -3.499999999999996003 ) ) ;
#5063 = FACE_OUTER_BOUND ( 'NONE', #7224, .T. ) ;
#5064 = CARTESIAN_POINT ( 'NONE',  ( -9.714451465470119729E-14, -4.618802153517051146, -0.5000000000000004441 ) ) ;
#5065 = DIRECTION ( 'NONE',  ( 2.220446049250313081E-16, -1.000000000000000000, 7.025792437124636392E-31 ) ) ;
#5066 = DIRECTION ( 'NONE',  ( 9.121204216617949000E-31, 1.000000000000000000, -6.982962677686261977E-15 ) ) ;
#5067 = CARTESIAN_POINT ( 'NONE',  ( 4.052424581287842997, -2.393186648133572625, 2.990837702970500445 ) ) ;
#5068 =( NAMED_UNIT ( * ) SI_UNIT ( $, .STERADIAN. ) SOLID_ANGLE_UNIT ( ) );
#5069 = ADVANCED_FACE ( 'NONE', ( #19121 ), #14759, .T. ) ;
#5070 = ADVANCED_FACE ( 'NONE', ( #4659 ), #3254, .T. ) ;
#5071 = B_SPLINE_CURVE_WITH_KNOTS ( 'NONE', 3,
 ( #9492, #14790, #7614, #18551, #18093, #21973, #16654, #566 ),
 .UNSPECIFIED., .F., .F.,
 ( 4, 2, 2, 4 ),
 ( 0.002775112046897002492, 0.003466237704215407826, 0.004157363361533813161, 0.005539614676170624696 ),
 .UNSPECIFIED. ) ;
#5072 = CARTESIAN_POINT ( 'NONE',  ( 0.000000000000000000, 2.775557561562891351E-14, 17.49999999999997513 ) ) ;
#5073 = ORIENTED_EDGE ( 'NONE', *, *, #21177, .T. ) ;
#5074 = AXIS2_PLACEMENT_3D ( 'NONE', #21045, #23045, #10678 ) ;
#5075 = CARTESIAN_POINT ( 'NONE',  ( -30.02510095774627530, 64.26821721294993495, 34.16570243528391160 ) ) ;
#5076 = AXIS2_PLACEMENT_3D ( 'NONE', #6164, #13563, #20866 ) ;
#5078 = ORIENTED_EDGE ( 'NONE', *, *, #3455, .F. ) ;
#5077 = VERTEX_POINT ( 'NONE', #10417 ) ;
#5079 = EDGE_CURVE ( 'NONE', #11319, #16591, #12502, .T. ) ;
#5080 = VERTEX_POINT ( 'NONE', #23010 ) ;
#5083 = ORIENTED_EDGE ( 'NONE', *, *, #3509, .F. ) ;
#5082 = EDGE_CURVE ( 'NONE', #23028, #13536, #19717, .T. ) ;
#5081 = ORIENTED_EDGE ( 'NONE', *, *, #3067, .T. ) ;
#5084 = DIRECTION ( 'NONE',  ( 1.333893503340774882E-15, 2.778352770573747380E-17, 1.000000000000000000 ) ) ;
#5085 = EDGE_CURVE ( 'NONE', #15653, #5583, #16624, .T. ) ;
#5086 = CARTESIAN_POINT ( 'NONE',  ( 2.775557561562891351E-14, 0.000000000000000000, -6.499999999999950262 ) ) ;
#5087 = CARTESIAN_POINT ( 'NONE',  ( -0.5000000000000975886, 1.999999999999890754, 7.500000000000007105 ) ) ;
#5088 = DIRECTION ( 'NONE',  ( 0.000000000000000000, 0.000000000000000000, 1.000000000000000000 ) ) ;
#5089 = LINE ( 'NONE', #17664, #17153 ) ;
#5090 = CARTESIAN_POINT ( 'NONE',  ( 112.6756160111034575, -11.28140466348828674, -6.500000000000040856 ) ) ;
#5091 = CARTESIAN_POINT ( 'NONE',  ( 35.50000000029184832, -9.961476088449217059E-10, -18.50000000000000355 ) ) ;
#5092 = DIRECTION ( 'NONE',  ( 1.550910762415566494E-16, 1.000000000000000000, -8.135128085091684243E-31 ) ) ;
#5093 = CARTESIAN_POINT ( 'NONE',  ( -3.999999999708153453, 35.99999999900384751, -19.50000000000000355 ) ) ;
#5094 = DIRECTION ( 'NONE',  ( -0.8660254037844401509, -0.4999999999999977240, 0.000000000000000000 ) ) ;
#5095 = CARTESIAN_POINT ( 'NONE',  ( 3.948095570617040639, 0.6965071952230758034, 3.499999999999995559 ) ) ;
#5096 = FACE_OUTER_BOUND ( 'NONE', #20280, .T. ) ;
#5097 = CARTESIAN_POINT ( 'NONE',  ( 7.500000000000007105, -1.999999999999991340, 11.74999999999998224 ) ) ;
#5098 = EDGE_CURVE ( 'NONE', #9917, #11317, #9118, .T. ) ;
#5099 = CIRCLE ( 'NONE', #10360, 3.000000000000011102 ) ;
#5100 = DIRECTION ( 'NONE',  ( 3.885780586188016830E-16, 4.437342591868156373E-31, -1.000000000000000000 ) ) ;
#5101 = DIRECTION ( 'NONE',  ( -1.000000000000000000, 0.000000000000000000, 0.000000000000000000 ) ) ;
#5102 = CARTESIAN_POINT ( 'NONE',  ( -9.714451465470119729E-14, -4.618802153517051146, -0.5000000000000004441 ) ) ;
#5103 = EDGE_LOOP ( 'NONE', ( #1044, #3324 ) ) ;
#5105 = VERTEX_POINT ( 'NONE', #18289 ) ;
#5104 = ORIENTED_EDGE ( 'NONE', *, *, #16137, .F. ) ;
#5106 = EDGE_CURVE ( 'NONE', #5668, #8762, #11141, .T. ) ;
#5107 = ORIENTED_EDGE ( 'NONE', *, *, #17085, .F. ) ;
#5108 = VERTEX_POINT ( 'NONE', #3596 ) ;
#5109 = ORIENTED_EDGE ( 'NONE', *, *, #3922, .F. ) ;
#5110 = EDGE_LOOP ( 'NONE', ( #13789, #10488, #14536, #1486 ) ) ;
#5111 = FACE_OUTER_BOUND ( 'NONE', #8816, .T. ) ;
#5112 = AXIS2_PLACEMENT_3D ( 'NONE', #16355, #256, #8854 ) ;
#5113 = DIRECTION ( 'NONE',  ( 0.000000000000000000, 0.000000000000000000, 1.000000000000000000 ) ) ;
#5114 = ORIENTED_EDGE ( 'NONE', *, *, #16858, .F. ) ;
#5115 = CARTESIAN_POINT ( 'NONE',  ( -50.65685424949274562, 7.200000000000025935, 17.71251237973613257 ) ) ;
#5116 = CARTESIAN_POINT ( 'NONE',  ( 57.15235153779116217, -1.074585193523325266, -5.999999999999894307 ) ) ;
#5117 = MECHANICAL_DESIGN_GEOMETRIC_PRESENTATION_REPRESENTATION (  '', ( #12233 ), #22025 ) ;
#5118 = DIRECTION ( 'NONE',  ( -1.000000000000000000, 1.771896121890576795E-14, -3.717264591378832268E-16 ) ) ;
#5119 = CARTESIAN_POINT ( 'NONE',  ( -95.70000000000069917, 2.700000000000014833, -2.000000000000001776 ) ) ;
#5120 = LINE ( 'NONE', #17699, #6897 ) ;
#5121 = PLANE ( 'NONE',  #4572 ) ;
#5122 = CARTESIAN_POINT ( 'NONE',  ( 12.84999999999997300, -1.999999999999998224, 0.000000000000000000 ) ) ;
#5123 = DIRECTION ( 'NONE',  ( 1.000000000000000000, 2.699383410053119644E-30, 3.330669073875432643E-16 ) ) ;
#5124 = CARTESIAN_POINT ( 'NONE',  ( 4.071447262713884463, 2.020725942163639655, -3.499999999999996003 ) ) ;
#5125 = CARTESIAN_POINT ( 'NONE',  ( 124.5000000000018332, -4.500000000000059508, -5.999999999999943157 ) ) ;
#5126 = FACE_OUTER_BOUND ( 'NONE', #14994, .T. ) ;
#5127 = EDGE_LOOP ( 'NONE', ( #13263, #19061 ) ) ;
#5128 = AXIS2_PLACEMENT_3D ( 'NONE', #9, #119, #21422 ) ;
#5129 = FILL_AREA_STYLE_COLOUR ( '', #19884 ) ;
#5130 = CARTESIAN_POINT ( 'NONE',  ( 4.175813232069142344, 4.122719923832743660, 0.000000000000000000 ) ) ;
#5131 = DIRECTION ( 'NONE',  ( -1.000000000000000000, -2.699383410053119644E-30, -3.330669073875432643E-16 ) ) ;
#5133 = ORIENTED_EDGE ( 'NONE', *, *, #7820, .F. ) ;
#5132 = ORIENTED_EDGE ( 'NONE', *, *, #12227, .F. ) ;
#5134 = EDGE_CURVE ( 'NONE', #1775, #1329, #21301, .T. ) ;
#5135 = AXIS2_PLACEMENT_3D ( 'NONE', #12789, #7504, #3963 ) ;
#5136 = ORIENTED_EDGE ( 'NONE', *, *, #8237, .T. ) ;
#5137 = AXIS2_PLACEMENT_3D ( 'NONE', #23228, #21576, #17806 ) ;
#5138 = VERTEX_POINT ( 'NONE', #3934 ) ;
#5139 = EDGE_CURVE ( 'NONE', #13451, #18021, #11104, .T. ) ;
#5140 = ORIENTED_EDGE ( 'NONE', *, *, #14573, .T. ) ;
#5141 = DIRECTION ( 'NONE',  ( -0.7313537016191735685, 0.6819983600624951459, -3.923113172947598083E-16 ) ) ;
#5142 = DIRECTION ( 'NONE',  ( -4.190823558986625216E-31, 1.000000000000000000, -4.190823558986625216E-31 ) ) ;
#5143 = CARTESIAN_POINT ( 'NONE',  ( 0.2499999999999932832, 2.775557561562891351E-14, -2.000000000000001776 ) ) ;
#5144 = CARTESIAN_POINT ( 'NONE',  ( -42.54314575050793934, 7.999999999999992895, 8.000000000000035527 ) ) ;
#5145 = LINE ( 'NONE', #17368, #7965 ) ;
#5146 = MANIFOLD_SOLID_BREP ( 'Cut-Extrude2', #6935 ) ;
#5147 = DIRECTION ( 'NONE',  ( 2.013525853228507892E-32, 6.902532920683810383E-31, -1.000000000000000000 ) ) ;
#5148 = DIRECTION ( 'NONE',  ( 1.000000000000000000, 0.000000000000000000, 0.000000000000000000 ) ) ;
#5149 = CARTESIAN_POINT ( 'NONE',  ( -8.233775472210618673, -0.5437072270125806739, 7.279685395985805663 ) ) ;
#5150 = DIRECTION ( 'NONE',  ( 0.000000000000000000, 1.000000000000000000, -0.000000000000000000 ) ) ;
#5151 = AXIS2_PLACEMENT_3D ( 'NONE', #9559, #13976, #22496 ) ;
#5152 = CARTESIAN_POINT ( 'NONE',  ( -6.999999999708142795, 49.99999999900385461, -18.99999999999998934 ) ) ;
#5153 = CARTESIAN_POINT ( 'NONE',  ( 0.000000000000000000, 0.000000000000000000, 0.000000000000000000 ) ) ;
#5154 = AXIS2_PLACEMENT_3D ( 'NONE', #6836, #8485, #8135 ) ;
#5155 = DIRECTION ( 'NONE',  ( -1.000000000000000000, -2.699383410053119644E-30, -3.330669073875432643E-16 ) ) ;
#5156 = TOROIDAL_SURFACE ( 'NONE', #18304, 6.500000000000000888, 0.5000000000000000000 ) ;
#5157 = DIRECTION ( 'NONE',  ( 0.000000000000000000, 0.000000000000000000, -1.000000000000000000 ) ) ;
#5158 = CARTESIAN_POINT ( 'NONE',  ( -2.807080416177946347, 3.225969019225889856, -3.502507215260549867 ) ) ;
#5159 = AXIS2_PLACEMENT_3D ( 'NONE', #10452, #23168, #9036 ) ;
#5160 = FACE_OUTER_BOUND ( 'NONE', #2059, .T. ) ;
#5161 = CARTESIAN_POINT ( 'NONE',  ( 118.0000000000019043, -7.000000000000006217, 6.500000000000103029 ) ) ;
#5162 = ORIENTED_EDGE ( 'NONE', *, *, #2459, .F. ) ;
#5163 = ORIENTED_EDGE ( 'NONE', *, *, #11403, .T. ) ;
#5164 = AXIS2_PLACEMENT_3D ( 'NONE', #9873, #7989, #20238 ) ;
#5165 = AXIS2_PLACEMENT_3D ( 'NONE', #3846, #21855, #5866 ) ;
#5166 = CARTESIAN_POINT ( 'NONE',  ( -6.605954977387137994, 35.99999999900384751, -26.25080446718044414 ) ) ;
#5168 = ORIENTED_EDGE ( 'NONE', *, *, #17211, .T. ) ;
#5167 = ORIENTED_EDGE ( 'NONE', *, *, #14686, .T. ) ;
#5169 = CIRCLE ( 'NONE', #17179, 0.5000000000000022204 ) ;
#5170 = CARTESIAN_POINT ( 'NONE',  ( -2.966164998648648687, -1.454929939081855750, -4.362451518707887388 ) ) ;
#5171 = CARTESIAN_POINT ( 'NONE',  ( -55.05572809000125289, 0.5000000000000143219, -10.00000000000006395 ) ) ;
#5172 =( LENGTH_UNIT ( ) NAMED_UNIT ( * ) SI_UNIT ( .MILLI., .METRE. ) );
#5173 = PRODUCT_RELATED_PRODUCT_CATEGORY ( 'part', '', ( #19447 ) ) ;
#5174 = CARTESIAN_POINT ( 'NONE',  ( -42.54314575050793934, -4.000000000000021316, 7.500000000000062172 ) ) ;
#5175 = AXIS2_PLACEMENT_3D ( 'NONE', #23231, #21347, #20030 ) ;
#5176 = EDGE_LOOP ( 'NONE', ( #3821, #21811, #2583, #6844 ) ) ;
#5177 = CARTESIAN_POINT ( 'NONE',  ( -5.773502691896283068, 4.999999999999979572, 4.999999999999997335 ) ) ;
#5178 = CARTESIAN_POINT ( 'NONE',  ( 3.951447005078446484, -2.357513599190976805, -2.916666666666666963 ) ) ;
#5179 = FACE_OUTER_BOUND ( 'NONE', #22067, .T. ) ;
#5180 = PRODUCT_DEFINITION_SHAPE ( 'NONE', 'NONE',  #23283 ) ;
#5181 = CARTESIAN_POINT ( 'NONE',  ( -6.000000000000047073, -4.800000000000006040, 8.000000000000090594 ) ) ;
#5182 = EDGE_CURVE ( 'NONE', #18271, #18021, #21529, .T. ) ;
#5183 = CARTESIAN_POINT ( 'NONE',  ( -42.54314575050785407, -4.000000000000021316, 8.000000000000007105 ) ) ;
#5184 = CARTESIAN_POINT ( 'NONE',  ( 4.000000000000007994, 8.673617379884035472E-16, -3.142992957459231462 ) ) ;
#5185 = LINE ( 'NONE', #10922, #8387 ) ;
#5186 = DIRECTION ( 'NONE',  ( -1.550910762415566494E-16, -1.000000000000000000, 8.135128085091684243E-31 ) ) ;
#5187 = FILL_AREA_STYLE_COLOUR ( '', #11535 ) ;
#5188 = AXIS2_PLACEMENT_3D ( 'NONE', #17559, #13806, #20990 ) ;
#5189 = MANIFOLD_SOLID_BREP ( 'Chamfer2', #6192 ) ;
#5190 = ADVANCED_FACE ( 'NONE', ( #9235 ), #294, .F. ) ;
#5191 = LINE ( 'NONE', #16344, #22862 ) ;
#5192 =( LENGTH_UNIT ( ) NAMED_UNIT ( * ) SI_UNIT ( .MILLI., .METRE. ) );
#5193 = ORIENTED_EDGE ( 'NONE', *, *, #8046, .T. ) ;
#5194 = AXIS2_PLACEMENT_3D ( 'NONE', #19161, #3173, #2692 ) ;
#5195 = CARTESIAN_POINT ( 'NONE',  ( -83.51225780769254925, 17.65948356667604102, 40.66570243528393291 ) ) ;
#5196 = AXIS2_PLACEMENT_3D ( 'NONE', #5302, #8949, #1989 ) ;
#5198 = ORIENTED_EDGE ( 'NONE', *, *, #9964, .T. ) ;
#5197 = ORIENTED_EDGE ( 'NONE', *, *, #12242, .T. ) ;
#5199 = ORIENTED_EDGE ( 'NONE', *, *, #20779, .T. ) ;
#5201 = ORIENTED_EDGE ( 'NONE', *, *, #9120, .T. ) ;
#5200 = EDGE_LOOP ( 'NONE', ( #8149, #1827, #20970, #2845 ) ) ;
#5202 = FACE_OUTER_BOUND ( 'NONE', #19169, .T. ) ;
#5203 = STYLED_ITEM ( 'NONE', ( #9734 ), #22653 ) ;
#5204 = PLANE ( 'NONE',  #22363 ) ;
#5205 = ADVANCED_FACE ( 'NONE', ( #5839 ), #18517, .T. ) ;
#5206 = CARTESIAN_POINT ( 'NONE',  ( 86.00000000000129319, -10.52760560296347947, 6.500000000000110134 ) ) ;
#5207 = DIRECTION ( 'NONE',  ( 0.000000000000000000, 6.802837160693368935E-15, 1.000000000000000000 ) ) ;
#5208 = ORIENTED_EDGE ( 'NONE', *, *, #13317, .F. ) ;
#5209 = DIRECTION ( 'NONE',  ( 1.000000000000000000, -4.190823558986621713E-31, 0.000000000000000000 ) ) ;
#5210 = CARTESIAN_POINT ( 'NONE',  ( -7.735962016526085172, -0.06991241830943269175, 7.174192622766982552 ) ) ;
#5211 =( BOUNDED_SURFACE ( )  B_SPLINE_SURFACE ( 3, 2, ( 
 ( #8455, #3278, #19151 ),
 ( #10324, #13631, #10445 ),
 ( #15381, #8331, #19379 ),
 ( #1509, #6578, #10102 ),
 ( #8223, #17495, #4797 ),
 ( #14089, #20825, #1168 ),
 ( #17372, #15496, #21043 ),
 ( #1285, #19260, #8568 ),
 ( #11968, #6926, #21276 ),
 ( #22569, #22925, #8679 ),
 ( #15614, #12313, #5149 ),
 ( #3398, #22806, #13749 ),
 ( #10203, #4688, #2924 ),
 ( #19502, #20930, #6687 ) ),
 .UNSPECIFIED., .F., .F., .T. ) 
 B_SPLINE_SURFACE_WITH_KNOTS ( ( 4, 2, 2, 2, 2, 2, 4 ),
 ( 3, 3 ),
 ( 1.951563910473907981E-18, 0.0009385527998839240113, 0.001407829199825884987, 0.001877105599767846071, 0.002346381999709806938, 0.002815658399651768239, 0.003754211199535690408 ),
 ( 0.000000000000000000, 1.000000000000000000 ),
 .UNSPECIFIED. ) 
 GEOMETRIC_REPRESENTATION_ITEM ( )  RATIONAL_B_SPLINE_SURFACE ( (
 ( 1.000000000000000000, 0.7071067811865440200, 1.000000000000000000),
 ( 1.000000000000000000, 0.7217349950159128724, 1.000000000000000000),
 ( 1.000000000000000000, 0.7325631490736875806, 1.000000000000000000),
 ( 1.000000000000000000, 0.7426392126583306608, 1.000000000000000000),
 ( 1.000000000000000000, 0.7449451721693339801, 1.000000000000000000),
 ( 1.000000000000000000, 0.7474053618999215720, 1.000000000000000000),
 ( 1.000000000000000000, 0.7475947887410936410, 1.000000000000000000),
 ( 1.000000000000000000, 0.7461109904164890949, 1.000000000000000000),
 ( 1.000000000000000000, 0.7444113185332733584, 1.000000000000000000),
 ( 1.000000000000000000, 0.7395217850810403837, 1.000000000000000000),
 ( 1.000000000000000000, 0.7363545993504035936, 1.000000000000000000),
 ( 1.000000000000000000, 0.7253814056385251563, 1.000000000000000000),
 ( 1.000000000000000000, 0.7159765610436893413, 1.000000000000000000),
 ( 1.000000000000000000, 0.7071067811865459074, 1.000000000000000000) ) ) 
 REPRESENTATION_ITEM ( '' )  SURFACE ( )  );
#5212 = PLANE ( 'NONE',  #18524 ) ;
#5213 = ADVANCED_FACE ( 'NONE', ( #2746 ), #4045, .F. ) ;
#5214 =( LENGTH_UNIT ( ) NAMED_UNIT ( * ) SI_UNIT ( .MILLI., .METRE. ) );
#5215 = AXIS2_PLACEMENT_3D ( 'NONE', #4777, #10305, #8201 ) ;
#5216 = CARTESIAN_POINT ( 'NONE',  ( -2.109645605488527628E-31, 1.750000000000001554, -2.500000000000000000 ) ) ;
#5217 = CARTESIAN_POINT ( 'NONE',  ( 66.26395429947838522, 0.000000000000000000, -6.499999999999859668 ) ) ;
#5218 = VECTOR ( 'NONE', #6349, 1000.000000000000000 ) ;
#5219 = TOROIDAL_SURFACE ( 'NONE', #8221, 7.208584908080424292, 5.000000000000000000 ) ;
#5220 = CARTESIAN_POINT ( 'NONE',  ( 36.00000000029184832, -9.961476088449217059E-10, -45.00000000000000000 ) ) ;
#5221 = CYLINDRICAL_SURFACE ( 'NONE', #8731, 2.999999999999995559 ) ;
#5222 = CARTESIAN_POINT ( 'NONE',  ( -3.999999999708139686, 49.99999999900386172, -15.99999999999999289 ) ) ;
#5223 = ADVANCED_FACE ( 'NONE', ( #11227 ), #5942, .T. ) ;
#5224 = FACE_OUTER_BOUND ( 'NONE', #12004, .T. ) ;
#5225 = EDGE_CURVE ( 'NONE', #12501, #4139, #6288, .T. ) ;
#5226 = CARTESIAN_POINT ( 'NONE',  ( -4.000000000000102141, 2.511478553582021433, -3.469254451724788524 ) ) ;
#5227 = CARTESIAN_POINT ( 'NONE',  ( -95.70000000000071338, 2.700000000000014833, 1.000000000000070166 ) ) ;
#5228 = ORIENTED_EDGE ( 'NONE', *, *, #12419, .F. ) ;
#5230 = VERTEX_POINT ( 'NONE', #6053 ) ;
#5229 = ORIENTED_EDGE ( 'NONE', *, *, #752, .F. ) ;
#5231 = VECTOR ( 'NONE', #22717, 1000.000000000000114 ) ;
#5232 = VERTEX_POINT ( 'NONE', #13461 ) ;
#5233 = AXIS2_PLACEMENT_3D ( 'NONE', #21953, #5845, #9127 ) ;
#5235 = VERTEX_POINT ( 'NONE', #12998 ) ;
#5234 = EDGE_LOOP ( 'NONE', ( #15456, #12007, #12891, #16771 ) ) ;
#5236 = AXIS2_PLACEMENT_3D ( 'NONE', #10182, #13834, #16992 ) ;
#5237 = ORIENTED_EDGE ( 'NONE', *, *, #7076, .F. ) ;
#5238 = EDGE_CURVE ( 'NONE', #1275, #21027, #18467, .T. ) ;
#5239 = VERTEX_POINT ( 'NONE', #20175 ) ;
#5240 = ADVANCED_FACE ( 'NONE', ( #16618 ), #13222, .T. ) ;
#5241 = DIRECTION ( 'NONE',  ( 1.000000000000000000, -4.615739097524200579E-16, -1.134196829589820086E-15 ) ) ;
#5242 = EDGE_CURVE ( 'NONE', #13739, #7712, #18979, .T. ) ;
#5243 = PLANE ( 'NONE',  #15126 ) ;
#5244 = EDGE_LOOP ( 'NONE', ( #16892, #23237 ) ) ;
#5245 = CARTESIAN_POINT ( 'NONE',  ( -65.00000000000046896, -0.5000000000000628386, 3.000000000000030198 ) ) ;
#5246 = DIRECTION ( 'NONE',  ( -1.000000000000000000, -4.440892098500626162E-16, 5.551115123125782702E-16 ) ) ;
#5247 = LINE ( 'NONE', #14179, #10999 ) ;
#5248 = CARTESIAN_POINT ( 'NONE',  ( -65.55642023346347003, -0.5000000000000628386, -11.87813525200320797 ) ) ;
#5249 = CARTESIAN_POINT ( 'NONE',  ( 0.1410422978105614067, -4.700232962125169500, -3.687027686973649132 ) ) ;
#5250 = DIRECTION ( 'NONE',  ( 1.000000000000000000, 0.000000000000000000, 0.000000000000000000 ) ) ;
#5251 = ADVANCED_FACE ( 'NONE', ( #9932 ), #470, .T. ) ;
#5252 = AXIS2_PLACEMENT_3D ( 'NONE', #3443, #164, #3737 ) ;
#5253 = DIRECTION ( 'NONE',  ( -1.000000000000000000, -6.938893903907186568E-15, 0.000000000000000000 ) ) ;
#5254 = EDGE_CURVE ( 'NONE', #15251, #14991, #18405, .T. ) ;
#5255 = CARTESIAN_POINT ( 'NONE',  ( -5.454524251050746564, 13.82936183575430356, -16.36878710987171459 ) ) ;
#5256 = VERTEX_POINT ( 'NONE', #11450 ) ;
#5257 =( NAMED_UNIT ( * ) SI_UNIT ( $, .STERADIAN. ) SOLID_ANGLE_UNIT ( ) );
#5258 = CARTESIAN_POINT ( 'NONE',  ( 37.43301270189239460, 0.2500000000000002220, -2.999999999999988898 ) ) ;
#5259 = LINE ( 'NONE', #1718, #17971 ) ;
#5260 = CONICAL_SURFACE ( 'NONE', #21025, 4.000000000000000000, 1.047197551196595855 ) ;
#5262 = ORIENTED_EDGE ( 'NONE', *, *, #6541, .F. ) ;
#5261 = EDGE_LOOP ( 'NONE', ( #6533, #2353, #5464, #4064 ) ) ;
#5263 = VERTEX_POINT ( 'NONE', #4384 ) ;
#5264 = ORIENTED_EDGE ( 'NONE', *, *, #217, .T. ) ;
#5265 = EDGE_LOOP ( 'NONE', ( #20009, #12578, #19806, #17128 ) ) ;
#5266 = LINE ( 'NONE', #23155, #20066 ) ;
#5267 = CARTESIAN_POINT ( 'NONE',  ( -4.113620667976075396, -1.750000000000001554, 2.374999999999986677 ) ) ;
#5268 = CARTESIAN_POINT ( 'NONE',  ( 3.878096787214412089, 2.680238624820988402, -2.357690525401514137 ) ) ;
#5269 = DIRECTION ( 'NONE',  ( -1.000000000000000000, 4.190823558986610327E-31, -1.733449886265890494E-32 ) ) ;
#5270 = CARTESIAN_POINT ( 'NONE',  ( 12.84999999999997300, -14.00000000000007105, 5.551115123125782702E-14 ) ) ;
#5271 = DIRECTION ( 'NONE',  ( -1.134196829589822256E-15, -2.220446049250322449E-16, 1.000000000000000000 ) ) ;
#5272 = AXIS2_PLACEMENT_3D ( 'NONE', #6425, #1016, #14916 ) ;
#5273 = DIRECTION ( 'NONE',  ( 2.013525853228507892E-32, 6.902532920683810383E-31, -1.000000000000000000 ) ) ;
#5274 = CARTESIAN_POINT ( 'NONE',  ( 2.499999999999998668, 2.000000000000001776, -18.75000000000001066 ) ) ;
#5275 = CARTESIAN_POINT ( 'NONE',  ( -3.200000000000091660, 5.299999999999998934, -8.000000000000035527 ) ) ;
#5276 = DIRECTION ( 'NONE',  ( -2.013525853228507892E-32, -6.902532920683810383E-31, 1.000000000000000000 ) ) ;
#5277 = CARTESIAN_POINT ( 'NONE',  ( -12.85000000000001386, -1.499999999999997780, -5.749999999999976907 ) ) ;
#5278 = DIRECTION ( 'NONE',  ( 1.550910762415566494E-16, 1.000000000000000000, -8.135128085091684243E-31 ) ) ;
#5279 = ADVANCED_FACE ( 'NONE', ( #14754 ), #4155, .T. ) ;
#5280 = CARTESIAN_POINT ( 'NONE',  ( -89.70000000000048601, -2.700000000000084110, 1.000000000000000888 ) ) ;
#5281 = CARTESIAN_POINT ( 'NONE',  ( 4.158807179406254662, 2.089320655794529191, -3.500000000000009326 ) ) ;
#5282 = ORIENTED_EDGE ( 'NONE', *, *, #2185, .F. ) ;
#5283 = CONTEXT_DEPENDENT_SHAPE_REPRESENTATION ( #22179, #13423 ) ;
#5284 = TOROIDAL_SURFACE ( 'NONE', #3034, 6.700000000000001066, 0.5000000000000000000 ) ;
#5285 = ORIENTED_EDGE ( 'NONE', *, *, #4036, .T. ) ;
#5286 = CARTESIAN_POINT ( 'NONE',  ( -6.231825765894918767, 35.99999999900384751, -26.01458861726397487 ) ) ;
#5288 = EDGE_LOOP ( 'NONE', ( #5586, #8419, #16769, #18267 ) ) ;
#5287 = ORIENTED_EDGE ( 'NONE', *, *, #3796, .F. ) ;
#5289 = CARTESIAN_POINT ( 'NONE',  ( 42.50000000000020606, 8.000000000000003553, 5.551115123125782702E-14 ) ) ;
#5290 = CARTESIAN_POINT ( 'NONE',  ( 59.19834661797866460, 1.119475911334100182, 6.500000000000130562 ) ) ;
#5291 = FACE_OUTER_BOUND ( 'NONE', #14629, .T. ) ;
#5292 = SURFACE_STYLE_USAGE ( .BOTH. , #16093 ) ;
#5293 = ORIENTED_EDGE ( 'NONE', *, *, #6066, .F. ) ;
#5294 = FACE_OUTER_BOUND ( 'NONE', #3994, .T. ) ;
#5295 = DIRECTION ( 'NONE',  ( 1.000000000000000000, -4.190823558986610327E-31, 1.733449886265890494E-32 ) ) ;
#5296 = DIRECTION ( 'NONE',  ( -5.598259082250079541E-17, 1.000000000000000000, -6.162975822039171151E-32 ) ) ;
#5297 = CARTESIAN_POINT ( 'NONE',  ( -6.000000000000116351, 1.999999999999960032, -7.500000000000062172 ) ) ;
#5298 = CARTESIAN_POINT ( 'NONE',  ( 4.175813232069149450, 2.061359961916364725, -3.570380186727398986 ) ) ;
#5299 = LINE ( 'NONE', #19886, #5557 ) ;
#5300 = VECTOR ( 'NONE', #17641, 1000.000000000000000 ) ;
#5301 = DIRECTION ( 'NONE',  ( 0.000000000000000000, 0.000000000000000000, 1.000000000000000000 ) ) ;
#5302 = CARTESIAN_POINT ( 'NONE',  ( 2.499999999999992006, 4.250000000000003553, -1.250000000000028866 ) ) ;
#5303 = CARTESIAN_POINT ( 'NONE',  ( 37.00000000000017053, 0.2500000000000002220, -2.566987298107781257 ) ) ;
#5304 = MANIFOLD_SOLID_BREP ( 'Fillet1', #14061 ) ;
#5305 = LINE ( 'NONE', #3427, #19852 ) ;
#5306 = DIRECTION ( 'NONE',  ( 1.000000000000000000, 0.000000000000000000, 0.000000000000000000 ) ) ;
#5307 = ORIENTED_EDGE ( 'NONE', *, *, #14027, .F. ) ;
#5308 = DIRECTION ( 'NONE',  ( -5.551115123125782702E-17, -1.665334536937734811E-16, -1.000000000000000000 ) ) ;
#5310 = ORIENTED_EDGE ( 'NONE', *, *, #21065, .T. ) ;
#5309 = ORIENTED_EDGE ( 'NONE', *, *, #22914, .T. ) ;
#5311 = ADVANCED_FACE ( 'NONE', ( #5096 ), #3477, .T. ) ;
#5312 = VERTEX_POINT ( 'NONE', #3103 ) ;
#5314 = ORIENTED_EDGE ( 'NONE', *, *, #13101, .T. ) ;
#5313 = ORIENTED_EDGE ( 'NONE', *, *, #2403, .T. ) ;
#5315 = CIRCLE ( 'NONE', #7202, 3.499999999999996003 ) ;
#5316 = CIRCLE ( 'NONE', #21486, 6.500000000000067502 ) ;
#5317 = CARTESIAN_POINT ( 'NONE',  ( -4.550510256924974684, 35.99999999900384751, -25.50000000000000000 ) ) ;
#5318 = DIRECTION ( 'NONE',  ( -1.000000000000000000, 1.276756478318923119E-15, -1.333893503340766797E-15 ) ) ;
#5319 = FACE_OUTER_BOUND ( 'NONE', #12052, .T. ) ;
#5320 = CARTESIAN_POINT ( 'NONE',  ( -12.85000000000001386, -12.00000000000006928, 4.163336342344337027E-14 ) ) ;
#5321 = CARTESIAN_POINT ( 'NONE',  ( 108.2426266706970637, -6.527605602963671316, -5.999999999999991118 ) ) ;
#5322 = CARTESIAN_POINT ( 'NONE',  ( -7.835312244869949261, -0.05103360697234399224, 7.041165740960511954 ) ) ;
#5323 = CARTESIAN_POINT ( 'NONE',  ( 7.523653856849481514, -12.92037830543529253, 8.801128846369500991 ) ) ;
#5324 = DIRECTION ( 'NONE',  ( -1.000000000000000000, 1.550910762415526064E-16, 0.000000000000000000 ) ) ;
#5325 = DIRECTION ( 'NONE',  ( 1.000000000000000000, 0.000000000000000000, 0.000000000000000000 ) ) ;
#5326 = CARTESIAN_POINT ( 'NONE',  ( 2.000000000000015543, -3.464101615137746837, 0.000000000000000000 ) ) ;
#5327 = FACE_OUTER_BOUND ( 'NONE', #1176, .T. ) ;
#5328 = EDGE_CURVE ( 'NONE', #3083, #8469, #12479, .T. ) ;
#5329 = CARTESIAN_POINT ( 'NONE',  ( 5.484827557301452217, -1.325747111984059590, 0.000000000000000000 ) ) ;
#5330 = CARTESIAN_POINT ( 'NONE',  ( 35.50000000029184832, 2.999999999003851503, -26.00000000000000000 ) ) ;
#5331 = CARTESIAN_POINT ( 'NONE',  ( 7.162073728446656240, -2.365283217609523092, 7.945145523438303492 ) ) ;
#5332 = AXIS2_PLACEMENT_3D ( 'NONE', #20900, #6892, #6430 ) ;
#5333 = TOROIDAL_SURFACE ( 'NONE', #1927, 1.750000000000000000, 0.2500000000000000000 ) ;
#5334 = DIRECTION ( 'NONE',  ( 0.000000000000000000, -1.000000000000000000, 0.000000000000000000 ) ) ;
#5335 = LINE ( 'NONE', #15789, #2509 ) ;
#5336 = ORIENTED_EDGE ( 'NONE', *, *, #21222, .F. ) ;
#5337 = ADVANCED_FACE ( 'NONE', ( #996 ), #20760, .F. ) ;
#5338 = FILL_AREA_STYLE_COLOUR ( '', #19135 ) ;
#5340 = ORIENTED_EDGE ( 'NONE', *, *, #10018, .T. ) ;
#5339 = VERTEX_POINT ( 'NONE', #4624 ) ;
#5341 = EDGE_CURVE ( 'NONE', #22506, #17475, #1950, .T. ) ;
#5342 = ORIENTED_EDGE ( 'NONE', *, *, #11839, .F. ) ;
#5344 = ORIENTED_EDGE ( 'NONE', *, *, #16549, .T. ) ;
#5343 = EDGE_LOOP ( 'NONE', ( #10627, #1078, #6817, #22910 ) ) ;
#5345 = AXIS2_PLACEMENT_3D ( 'NONE', #4742, #10382, #17554 ) ;
#5346 =( REPRESENTATION_RELATIONSHIP ('NONE','NONE', #19450, #1856 ) REPRESENTATION_RELATIONSHIP_WITH_TRANSFORMATION ( #6007 )SHAPE_REPRESENTATION_RELATIONSHIP( ) );
#5347 = ORIENTED_EDGE ( 'NONE', *, *, #2196, .T. ) ;
#5348 = ORIENTED_EDGE ( 'NONE', *, *, #368, .F. ) ;
#5349 = VERTEX_POINT ( 'NONE', #22630 ) ;
#5350 = LINE ( 'NONE', #22888, #17427 ) ;
#5351 = EDGE_CURVE ( 'NONE', #10626, #93, #7976, .T. ) ;
#5352 = TOROIDAL_SURFACE ( 'NONE', #8346, 4.500000000000000888, 0.5000000000000000000 ) ;
#5353 = EDGE_CURVE ( 'NONE', #9565, #21352, #15784, .T. ) ;
#5354 = B_SPLINE_CURVE_WITH_KNOTS ( 'NONE', 3,
 ( #14950, #12964, #12842, #2480, #20367, #844 ),
 .UNSPECIFIED., .F., .F.,
 ( 4, 2, 4 ),
 ( 0.007276530541002032039, 0.009452065467417725131, 0.01162760039383341909 ),
 .UNSPECIFIED. ) ;
#5355 = PLANE ( 'NONE',  #1975 ) ;
#5356 = CYLINDRICAL_SURFACE ( 'NONE', #15392, 2.550000000000002043 ) ;
#5357 = EDGE_CURVE ( 'NONE', #6270, #1104, #2707, .T. ) ;
#5358 = AXIS2_PLACEMENT_3D ( 'NONE', #14441, #16183, #21512 ) ;
#5359 = FACE_OUTER_BOUND ( 'NONE', #22387, .T. ) ;
#5360 = DIRECTION ( 'NONE',  ( 1.454462294001240516E-30, 1.000000000000000000, 0.000000000000000000 ) ) ;
#5361 = DIRECTION ( 'NONE',  ( -1.000000000000000000, -1.479114197289397135E-31, -5.916456789157588541E-31 ) ) ;
#5362 = CARTESIAN_POINT ( 'NONE',  ( -4.024497503033621193, 2.323544716729374571, -3.572167766733397976 ) ) ;
#5363 =( NAMED_UNIT ( * ) PLANE_ANGLE_UNIT ( ) SI_UNIT ( $, .RADIAN. ) );
#5364 = CARTESIAN_POINT ( 'NONE',  ( -67.28510754798023186, 2.700000000000021938, 12.22107821754961421 ) ) ;
#5365 = AXIS2_PLACEMENT_3D ( 'NONE', #18989, #6861, #3344 ) ;
#5366 = CARTESIAN_POINT ( 'NONE',  ( -5.281014309470091206, 13.78823385074812613, -16.28034847426729925 ) ) ;
#5367 = B_SPLINE_CURVE_WITH_KNOTS ( 'NONE', 3,
 ( #22272, #6168, #11559, #6278, #8501, #10150 ),
 .UNSPECIFIED., .F., .F.,
 ( 4, 2, 4 ),
 ( 0.000000000000000000, 0.0002095117440854730941, 0.0004190234881709461881 ),
 .UNSPECIFIED. ) ;
#5368 = CARTESIAN_POINT ( 'NONE',  ( -7.764145988665025477, -1.774864566462279081, 8.011880279048810394 ) ) ;
#5369 = EDGE_CURVE ( 'NONE', #8601, #5408, #22867, .T. ) ;
#5370 = ORIENTED_EDGE ( 'NONE', *, *, #11976, .T. ) ;
#5371 = EDGE_CURVE ( 'NONE', #19811, #16509, #20365, .T. ) ;
#5372 = CARTESIAN_POINT ( 'NONE',  ( 2.918498775983380256E-10, 2.999999999003851503, -32.00000000000000000 ) ) ;
#5373 = DIRECTION ( 'NONE',  ( -1.214306433183769502E-15, -6.741645191078037727E-32, 1.000000000000000000 ) ) ;
#5374 = CIRCLE ( 'NONE', #18881, 6.249999999999992006 ) ;
#5376 = ORIENTED_EDGE ( 'NONE', *, *, #21205, .T. ) ;
#5375 = EDGE_LOOP ( 'NONE', ( #13847, #10335, #11434, #6875 ) ) ;
#5377 = CIRCLE ( 'NONE', #21142, 6.000000000000023093 ) ;
#5378 = AXIS2_PLACEMENT_3D ( 'NONE', #14750, #14870, #12635 ) ;
#5379 = CIRCLE ( 'NONE', #20008, 0.5000000000000017764 ) ;
#5380 = ORIENTED_EDGE ( 'NONE', *, *, #586, .F. ) ;
#5381 = ORIENTED_EDGE ( 'NONE', *, *, #6980, .F. ) ;
#5383 = ORIENTED_EDGE ( 'NONE', *, *, #20439, .T. ) ;
#5382 = EDGE_CURVE ( 'NONE', #12862, #4498, #14352, .T. ) ;
#5384 = VERTEX_POINT ( 'NONE', #19439 ) ;
#5385 = DIRECTION ( 'NONE',  ( 1.000000000000000000, 0.000000000000000000, 0.000000000000000000 ) ) ;
#5386 = EDGE_CURVE ( 'NONE', #4400, #4523, #2343, .T. ) ;
#5387 = CARTESIAN_POINT ( 'NONE',  ( 0.9337610950194882298, 1.709055944985350850, 4.749999999999999112 ) ) ;
#5388 = CARTESIAN_POINT ( 'NONE',  ( 3.972066048304740971, 2.740530939476234717, -2.384802634787816178 ) ) ;
#5389 = EDGE_CURVE ( 'NONE', #20148, #20452, #3831, .T. ) ;
#5390 = CARTESIAN_POINT ( 'NONE',  ( 4.175813232069149450, -4.122719923832729449, 0.000000000000000000 ) ) ;
#5391 = TOROIDAL_SURFACE ( 'NONE', #8812, 0.7500000000000000000, 0.2500000000000000000 ) ;
#5392 = DIRECTION ( 'NONE',  ( 1.000000000000000000, 2.168404344970991858E-16, 5.348730717595112872E-15 ) ) ;
#5393 = AXIS2_PLACEMENT_3D ( 'NONE', #21794, #7771, #16808 ) ;
#5394 = DIRECTION ( 'NONE',  ( 1.000000000000000000, 0.000000000000000000, 0.000000000000000000 ) ) ;
#5395 = CARTESIAN_POINT ( 'NONE',  ( 7.500000000000007105, -11.35410196624971491, 9.250000000000021316 ) ) ;
#5396 = CARTESIAN_POINT ( 'NONE',  ( -47.47487373415321343, -4.018019484660590557, 7.500000000000062172 ) ) ;
#5397 = VECTOR ( 'NONE', #10147, 1000.000000000000000 ) ;
#5398 = DIRECTION ( 'NONE',  ( 8.438582421954110511E-32, 0.000000000000000000, 1.000000000000000000 ) ) ;
#5399 = CARTESIAN_POINT ( 'NONE',  ( 37.54332536350037230, 10.88440674090231752, -10.22062532321614192 ) ) ;
#5400 = DIRECTION ( 'NONE',  ( 0.000000000000000000, -1.000000000000000000, 0.000000000000000000 ) ) ;
#5401 = FACE_OUTER_BOUND ( 'NONE', #423, .T. ) ;
#5402 = DIRECTION ( 'NONE',  ( -1.000000000000000000, 4.437342591868175641E-31, -3.330669073875457788E-16 ) ) ;
#5403 = CARTESIAN_POINT ( 'NONE',  ( 0.000000000000000000, 0.000000000000000000, -4.484454397937119197 ) ) ;
#5404 = DIRECTION ( 'NONE',  ( -1.000000000000000000, -4.440892098500626162E-16, 5.551115123125782702E-16 ) ) ;
#5405 = EDGE_LOOP ( 'NONE', ( #17117, #20813, #1067, #4675 ) ) ;
#5406 = VECTOR ( 'NONE', #5035, 1000.000000000000000 ) ;
#5407 = AXIS2_PLACEMENT_3D ( 'NONE', #20110, #7526, #5999 ) ;
#5408 = VERTEX_POINT ( 'NONE', #13694 ) ;
#5409 = CIRCLE ( 'NONE', #10649, 4.000000000000023981 ) ;
#5410 = EDGE_CURVE ( 'NONE', #1155, #13674, #17084, .T. ) ;
#5411 = CIRCLE ( 'NONE', #1660, 0.5000000000000031086 ) ;
#5412 = AXIS2_PLACEMENT_3D ( 'NONE', #16667, #16437, #20334 ) ;
#5413 = DIRECTION ( 'NONE',  ( -2.013525853228507892E-32, -6.902532920683810383E-31, 1.000000000000000000 ) ) ;
#5414 = ORIENTED_EDGE ( 'NONE', *, *, #11782, .T. ) ;
#5415 = ADVANCED_FACE ( 'NONE', ( #15330 ), #15472, .F. ) ;
#5416 = CARTESIAN_POINT ( 'NONE',  ( -4.113620667976089607, -1.750000000000001554, -2.375000000000005773 ) ) ;
#5417 = LINE ( 'NONE', #1527, #17510 ) ;
#5418 = ADVANCED_FACE ( 'NONE', ( #3227, #11910 ), #6406, .F. ) ;
#5419 = CARTESIAN_POINT ( 'NONE',  ( 8.438463404362677167, -11.99816466695113881, 6.398712851742227592 ) ) ;
#5420 = CARTESIAN_POINT ( 'NONE',  ( 25.60000000000000142, 6.951083313223974888E-32, 2.054999999999995719 ) ) ;
#5421 = EDGE_LOOP ( 'NONE', ( #10520, #14771, #4286, #4710 ) ) ;
#5422 = FACE_OUTER_BOUND ( 'NONE', #22497, .T. ) ;
#5423 = CARTESIAN_POINT ( 'NONE',  ( -1.839530896101882362, -1.562503694756887995, -4.750000000000026645 ) ) ;
#5424 = LINE ( 'NONE', #1868, #15791 ) ;
#5425 = LINE ( 'NONE', #3648, #3138 ) ;
#5426 = DIRECTION ( 'NONE',  ( 1.000000000000000000, 3.254448077276381206E-32, 1.066788928082016908E-26 ) ) ;
#5427 = CARTESIAN_POINT ( 'NONE',  ( 7.000000000000006217, -0.9711575687493152476, 9.522727272727294690 ) ) ;
#5428 = AXIS2_PLACEMENT_3D ( 'NONE', #17670, #162, #12609 ) ;
#5429 = CARTESIAN_POINT ( 'NONE',  ( 4.124214193018077346, 2.028338413290940778, -3.513185186763563728 ) ) ;
#5430 = CARTESIAN_POINT ( 'NONE',  ( 4.180231891692627322, -4.134807952925598329, -0.02076457676761531146 ) ) ;
#5431 = AXIS2_PLACEMENT_3D ( 'NONE', #18886, #22184, #6069 ) ;
#5432 = CARTESIAN_POINT ( 'NONE',  ( 4.071447262713884463, -4.041451884327383226, 0.000000000000000000 ) ) ;
#5433 = ORIENTED_EDGE ( 'NONE', *, *, #16391, .T. ) ;
#5434 = SHAPE_DEFINITION_REPRESENTATION ( #19249, #20536 ) ;
#5436 = EDGE_LOOP ( 'NONE', ( #12421, #18694, #19455, #8267 ) ) ;
#5435 = EDGE_LOOP ( 'NONE', ( #14285, #12987, #7056, #1885, #22393, #1297 ) ) ;
#5437 = EDGE_CURVE ( 'NONE', #17782, #7940, #6601, .T. ) ;
#5438 = VERTEX_POINT ( 'NONE', #9206 ) ;
#5439 = AXIS2_PLACEMENT_3D ( 'NONE', #260, #13192, #7774 ) ;
#5441 = ORIENTED_EDGE ( 'NONE', *, *, #5944, .T. ) ;
#5440 = VERTEX_POINT ( 'NONE', #6994 ) ;
#5442 = AXIS2_PLACEMENT_3D ( 'NONE', #1195, #18959, #20957 ) ;
#5443 = DIRECTION ( 'NONE',  ( 1.333893503340774882E-15, 2.778352770573747380E-17, 1.000000000000000000 ) ) ;
#5444 = AXIS2_PLACEMENT_3D ( 'NONE', #22157, #754, #7806 ) ;
#5445 = ADVANCED_FACE ( 'NONE', ( #16363 ), #16132, .F. ) ;
#5446 = CARTESIAN_POINT ( 'NONE',  ( 7.271441198316225041, -0.2709289393878955843, 8.039702399269760491 ) ) ;
#5447 =( NAMED_UNIT ( * ) SI_UNIT ( $, .STERADIAN. ) SOLID_ANGLE_UNIT ( ) );
#5448 = CARTESIAN_POINT ( 'NONE',  ( 6.000000000291855429, -9.961476088449217059E-10, -36.44999999999999574 ) ) ;
#5449 = CARTESIAN_POINT ( 'NONE',  ( 12.84999999999997300, -1.999999999999998224, 0.000000000000000000 ) ) ;
#5450 = CARTESIAN_POINT ( 'NONE',  ( 2.085593006335308133E-14, 10.00000000000000533, -2.500000000000000000 ) ) ;
#5451 = DIRECTION ( 'NONE',  ( -0.9706398123736329486, 1.505375731439247187E-16, -0.2405376366294442458 ) ) ;
#5452 = DIRECTION ( 'NONE',  ( -1.000000000000000000, 1.369518533665891191E-16, -1.780374093765658523E-15 ) ) ;
#5453 = CARTESIAN_POINT ( 'NONE',  ( 0.000000000000000000, 0.000000000000000000, -5.600000000000000533 ) ) ;
#5454 = FACE_OUTER_BOUND ( 'NONE', #657, .T. ) ;
#5455 = EDGE_CURVE ( 'NONE', #10365, #16744, #21511, .T. ) ;
#5456 = DIRECTION ( 'NONE',  ( -1.000000000000000000, -6.224605580259554159E-31, 2.887593071917436153E-31 ) ) ;
#5457 = AXIS2_PLACEMENT_3D ( 'NONE', #21658, #19531, #3310 ) ;
#5458 = DIRECTION ( 'NONE',  ( -7.860214984770699307E-18, 1.409037165336591006E-16, 1.000000000000000000 ) ) ;
#5459 = CARTESIAN_POINT ( 'NONE',  ( 7.282868595548843693, -0.2617430505219933701, 8.010178330700751914 ) ) ;
#5460 = ORIENTED_EDGE ( 'NONE', *, *, #22711, .F. ) ;
#5461 = PRESENTATION_STYLE_ASSIGNMENT (( #12618 ) ) ;
#5463 = ORIENTED_EDGE ( 'NONE', *, *, #21283, .T. ) ;
#5462 = EDGE_LOOP ( 'NONE', ( #12391, #3575 ) ) ;
#5464 = ORIENTED_EDGE ( 'NONE', *, *, #2608, .F. ) ;
#5466 = EDGE_LOOP ( 'NONE', ( #19541, #5133, #6353, #22188 ) ) ;
#5465 = VERTEX_POINT ( 'NONE', #8740 ) ;
#5467 = ORIENTED_EDGE ( 'NONE', *, *, #21293, .F. ) ;
#5468 = ORIENTED_EDGE ( 'NONE', *, *, #10075, .F. ) ;
#5469 = EDGE_LOOP ( 'NONE', ( #11756, #4838, #4003, #3949 ) ) ;
#5470 = LINE ( 'NONE', #5929, #10298 ) ;
#5471 = AXIS2_PLACEMENT_3D ( 'NONE', #5033, #10559, #12315 ) ;
#5472 = CIRCLE ( 'NONE', #6224, 4.000000000000023981 ) ;
#5473 = DIRECTION ( 'NONE',  ( 2.775557561562886729E-17, -4.401632478328199173E-16, 1.000000000000000000 ) ) ;
#5474 = DIRECTION ( 'NONE',  ( 0.000000000000000000, 0.000000000000000000, 1.000000000000000000 ) ) ;
#5475 = DIRECTION ( 'NONE',  ( 0.7071067811865475727, 0.7071067811865475727, 0.000000000000000000 ) ) ;
#5476 = CARTESIAN_POINT ( 'NONE',  ( 4.142654963991851957, -2.035398498734401596, -3.525413613457302198 ) ) ;
#5477 = DIRECTION ( 'NONE',  ( 1.066786462891689527E-26, 6.656013887802287108E-31, 1.000000000000000000 ) ) ;
#5478 = CYLINDRICAL_SURFACE ( 'NONE', #23055, 0.5000000000000038858 ) ;
#5479 = DIRECTION ( 'NONE',  ( -1.550910762415566494E-16, -1.000000000000000000, 8.135128085091684243E-31 ) ) ;
#5480 = EDGE_CURVE ( 'NONE', #20423, #20045, #17349, .T. ) ;
#5481 = DIRECTION ( 'NONE',  ( 0.5000000000000047740, 0.8660254037844359321, 6.910079924703084860E-16 ) ) ;
#5482 = CIRCLE ( 'NONE', #13740, 0.5000000000000039968 ) ;
#5483 = CARTESIAN_POINT ( 'NONE',  ( -6.000000000000116351, 1.999999999999960032, -7.500000000000062172 ) ) ;
#5484 = CARTESIAN_POINT ( 'NONE',  ( 3.973110223767149840, -2.262799480050941678E-11, -3.565797985667468417 ) ) ;
#5485 = ORIENTED_EDGE ( 'NONE', *, *, #12201, .T. ) ;
#5486 = EDGE_CURVE ( 'NONE', #14699, #1834, #21801, .T. ) ;
#5487 =( NAMED_UNIT ( * ) PLANE_ANGLE_UNIT ( ) SI_UNIT ( $, .RADIAN. ) );
#5488 = CARTESIAN_POINT ( 'NONE',  ( 12.84999999999997300, -12.00000000000011191, -5.749999999999936051 ) ) ;
#5490 = ORIENTED_EDGE ( 'NONE', *, *, #15626, .F. ) ;
#5489 = ORIENTED_EDGE ( 'NONE', *, *, #10925, .T. ) ;
#5491 = EDGE_CURVE ( 'NONE', #5891, #396, #1593, .T. ) ;
#5492 = ORIENTED_EDGE ( 'NONE', *, *, #12669, .F. ) ;
#5493 = VERTEX_POINT ( 'NONE', #21575 ) ;
#5494 = ORIENTED_EDGE ( 'NONE', *, *, #9228, .T. ) ;
#5495 = AXIS2_PLACEMENT_3D ( 'NONE', #8462, #22702, #20831 ) ;
#5496 = CARTESIAN_POINT ( 'NONE',  ( 88.75737332930592061, -6.527605602963476805, -6.000000000000012434 ) ) ;
#5497 = PLANE ( 'NONE',  #19245 ) ;
#5498 = FACE_OUTER_BOUND ( 'NONE', #20907, .T. ) ;
#5499 = CARTESIAN_POINT ( 'NONE',  ( 4.142654963991857286, -2.035398498734348305, -3.525413613457310635 ) ) ;
#5500 = ADVANCED_FACE ( 'NONE', ( #7445 ), #17918, .T. ) ;
#5501 = LINE ( 'NONE', #3163, #12872 ) ;
#5502 = DIRECTION ( 'NONE',  ( -1.000000000000000000, -4.440892098500626162E-16, 5.551115123125782702E-16 ) ) ;
#5503 = CARTESIAN_POINT ( 'NONE',  ( 0.000000000000000000, 1.750000000000001554, 0.000000000000000000 ) ) ;
#5504 = CARTESIAN_POINT ( 'NONE',  ( 9.184850986335003870E-16, 4.472790346437877718E-27, 7.499999999999998224 ) ) ;
#5505 = ADVANCED_FACE ( 'NONE', ( #21344 ), #18872, .F. ) ;
#5506 = CARTESIAN_POINT ( 'NONE',  ( -7.132286784435623694, -13.57635026841689019, 8.470912490188640120 ) ) ;
#5507 = DIRECTION ( 'NONE',  ( 0.7071067811865474617, -0.7071067811865474617, 0.000000000000000000 ) ) ;
#5508 = VECTOR ( 'NONE', #21760, 1000.000000000000000 ) ;
#5509 = CARTESIAN_POINT ( 'NONE',  ( -55.05572809000125289, -1.040834085586084257E-13, -10.00000000000006395 ) ) ;
#5510 = DIRECTION ( 'NONE',  ( -1.000000000000000000, 4.615739097524200579E-16, 1.134196829589820086E-15 ) ) ;
#5511 = CARTESIAN_POINT ( 'NONE',  ( -7.938566201357386554, 4.882486540518891971, 1.249999999999988898 ) ) ;
#5512 = AXIS2_PLACEMENT_3D ( 'NONE', #16534, #14669, #21852 ) ;
#5513 = EDGE_CURVE ( 'NONE', #14796, #7570, #17805, .T. ) ;
#5514 = CARTESIAN_POINT ( 'NONE',  ( 0.2500000000000140998, 1.250000000000015099, 0.000000000000000000 ) ) ;
#5515 = PLANE ( 'NONE',  #1048 ) ;
#5516 = ADVANCED_FACE ( 'NONE', ( #14499 ), #5221, .F. ) ;
#5517 = ORIENTED_EDGE ( 'NONE', *, *, #20768, .F. ) ;
#5518 = ADVANCED_FACE ( 'NONE', ( #5454 ), #17746, .T. ) ;
#5519 = ORIENTED_EDGE ( 'NONE', *, *, #15983, .T. ) ;
#5520 = CARTESIAN_POINT ( 'NONE',  ( -6.938893903907228378E-14, 4.999999999999976907, -4.163336342344337027E-14 ) ) ;
#5521 = ORIENTED_EDGE ( 'NONE', *, *, #9147, .T. ) ;
#5522 = AXIS2_PLACEMENT_3D ( 'NONE', #16181, #7267, #10781 ) ;
#5523 = ADVANCED_FACE ( 'NONE', ( #3783 ), #10604, .T. ) ;
#5524 = DIRECTION ( 'NONE',  ( -3.241725282392603095E-30, -1.000000000000000000, 2.218671295934100958E-31 ) ) ;
#5525 = CARTESIAN_POINT ( 'NONE',  ( 2.499999999999960476, 4.250000000000017764, -18.75000000000002132 ) ) ;
#5526 = ADVANCED_FACE ( 'NONE', ( #17671 ), #1562, .F. ) ;
#5527 = CARTESIAN_POINT ( 'NONE',  ( 7.162073728446673115, -11.63471678239051954, 7.945145523438290169 ) ) ;
#5528 = AXIS2_PLACEMENT_3D ( 'NONE', #4975, #15672, #6868 ) ;
#5529 = DIRECTION ( 'NONE',  ( -1.000000000000000000, -1.479114197289397135E-31, -5.916456789157588541E-31 ) ) ;
#5530 = EDGE_CURVE ( 'NONE', #4164, #2826, #1967, .T. ) ;
#5531 = ORIENTED_EDGE ( 'NONE', *, *, #11979, .F. ) ;
#5532 = PLANE ( 'NONE',  #7275 ) ;
#5533 = DIRECTION ( 'NONE',  ( -5.551115123125818447E-17, -6.982962677686276177E-15, -1.000000000000000000 ) ) ;
#5534 = CARTESIAN_POINT ( 'NONE',  ( 42.50000000000014921, 2.499999999999995115, -0.4999999999999726885 ) ) ;
#5535 = CARTESIAN_POINT ( 'NONE',  ( 8.697224362267997222, -14.00000000000004974, 6.250000000000033751 ) ) ;
#5536 = DIRECTION ( 'NONE',  ( -2.013525853228507892E-32, -6.902532920683810383E-31, 1.000000000000000000 ) ) ;
#5537 = CARTESIAN_POINT ( 'NONE',  ( 0.000000000000000000, -14.99999999999997513, -1.387778780781445676E-14 ) ) ;
#5538 = DIRECTION ( 'NONE',  ( 0.7071067811865524577, 0.7071067811865425767, 2.121016688166341246E-16 ) ) ;
#5539 = CARTESIAN_POINT ( 'NONE',  ( 54.42435809754109499, 0.000000000000000000, 6.500000000000144773 ) ) ;
#5540 = ADVANCED_FACE ( 'NONE', ( #7215 ), #14379, .T. ) ;
#5541 = DIRECTION ( 'NONE',  ( 0.000000000000000000, 0.000000000000000000, -1.000000000000000000 ) ) ;
#5542 = MANIFOLD_SOLID_BREP ( 'Chamfer1', #15926 ) ;
#5543 = EDGE_CURVE ( 'NONE', #17281, #3485, #7671, .T. ) ;
#5544 = DIRECTION ( 'NONE',  ( 0.4999999999999999445, 4.767331059895059913E-16, 0.8660254037844387076 ) ) ;
#5545 = ORIENTED_EDGE ( 'NONE', *, *, #10091, .F. ) ;
#5546 = VECTOR ( 'NONE', #6005, 1000.000000000000000 ) ;
#5547 = SHAPE_DEFINITION_REPRESENTATION ( #15290, #981 ) ;
#5549 = ORIENTED_EDGE ( 'NONE', *, *, #18330, .F. ) ;
#5548 = ORIENTED_EDGE ( 'NONE', *, *, #5782, .F. ) ;
#5550 = TOROIDAL_SURFACE ( 'NONE', #21346, 9.499999999999998224, 0.5000000000000000000 ) ;
#5552 = VERTEX_POINT ( 'NONE', #11422 ) ;
#5551 = ORIENTED_EDGE ( 'NONE', *, *, #22752, .F. ) ;
#5553 = CARTESIAN_POINT ( 'NONE',  ( 2.836893136758258382, 3.208949435746023315, -3.505054077164891257 ) ) ;
#5554 = LINE ( 'NONE', #376, #1325 ) ;
#5555 = CARTESIAN_POINT ( 'NONE',  ( 7.521298409251910400, -11.75792766829873237, 8.817899680514896588 ) ) ;
#5556 = CARTESIAN_POINT ( 'NONE',  ( -8.079084010241061264, -11.97965595983265530, 6.665520415301771529 ) ) ;
#5557 = VECTOR ( 'NONE', #12585, 1000.000000000000000 ) ;
#5558 = CARTESIAN_POINT ( 'NONE',  ( -6.245004513516505540E-14, -4.862606272033144883, -3.745885042887461935 ) ) ;
#5559 = CARTESIAN_POINT ( 'NONE',  ( 1.999999999999974021, 3.464101615137785029, 3.469446951953614189E-15 ) ) ;
#5560 = AXIS2_PLACEMENT_3D ( 'NONE', #12146, #5334, #19336 ) ;
#5561 = FACE_OUTER_BOUND ( 'NONE', #5851, .T. ) ;
#5562 = FACE_OUTER_BOUND ( 'NONE', #3295, .T. ) ;
#5563 = CARTESIAN_POINT ( 'NONE',  ( -6.999999999708142795, 49.99999999900385461, -18.99999999999998934 ) ) ;
#5564 = CYLINDRICAL_SURFACE ( 'NONE', #5428, 4.750000000000013323 ) ;
#5565 = CIRCLE ( 'NONE', #15302, 2.500000000000003997 ) ;
#5566 = CARTESIAN_POINT ( 'NONE',  ( 25.00000000000000355, 2.000000000000001776, -2.000000000000005329 ) ) ;
#5567 = DIRECTION ( 'NONE',  ( -1.454462294001240516E-30, -1.000000000000000000, -0.000000000000000000 ) ) ;
#5568 = AXIS2_PLACEMENT_3D ( 'NONE', #17894, #21777, #5544 ) ;
#5569 = CARTESIAN_POINT ( 'NONE',  ( 54.42435809754108078, -4.000000000000003553, 6.500000000000081712 ) ) ;
#5570 = CIRCLE ( 'NONE', #14579, 6.500000000000000888 ) ;
#5571 = CARTESIAN_POINT ( 'NONE',  ( 33.59619407800440882, 21.59619407671641866, -26.50000000000000000 ) ) ;
#5572 = CARTESIAN_POINT ( 'NONE',  ( 7.920269128372694922, -0.6322607639407502589, 7.713069291591495791 ) ) ;
#5573 = CIRCLE ( 'NONE', #18705, 9.000000000000031974 ) ;
#5574 = EDGE_CURVE ( 'NONE', #19243, #12740, #7898, .T. ) ;
#5575 = ORIENTED_EDGE ( 'NONE', *, *, #14407, .F. ) ;
#5576 = B_SPLINE_CURVE_WITH_KNOTS ( 'NONE', 3,
 ( #7221, #12735, #10956, #4130, #2025, #9211, #3683, #14385 ),
 .UNSPECIFIED., .F., .F.,
 ( 4, 2, 2, 4 ),
 ( 2.405267759940038380E-17, 0.001312337235399278637, 0.001968505853098905922, 0.002624674470798532989 ),
 .UNSPECIFIED. ) ;
#5578 = ORIENTED_EDGE ( 'NONE', *, *, #20728, .T. ) ;
#5577 = ORIENTED_EDGE ( 'NONE', *, *, #11369, .F. ) ;
#5579 = UNCERTAINTY_MEASURE_WITH_UNIT (LENGTH_MEASURE( 1.000000000000000082E-05 ), #6129, 'distance_accuracy_value', 'NONE');
#5580 = VECTOR ( 'NONE', #18612, 1000.000000000000000 ) ;
#5581 = MANIFOLD_SOLID_BREP ( 'Chamfer1', #4672 ) ;
#5582 = ORIENTED_EDGE ( 'NONE', *, *, #17415, .F. ) ;
#5584 = ORIENTED_EDGE ( 'NONE', *, *, #11690, .T. ) ;
#5583 = VERTEX_POINT ( 'NONE', #2369 ) ;
#5585 = CONICAL_SURFACE ( 'NONE', #11576, 5.371010071662839280, 1.221730476396037490 ) ;
#5586 = ORIENTED_EDGE ( 'NONE', *, *, #9228, .F. ) ;
#5587 = CARTESIAN_POINT ( 'NONE',  ( 4.071447262713884463, 2.020725942163688504, 3.499999999999997780 ) ) ;
#5588 = ORIENTED_EDGE ( 'NONE', *, *, #16336, .T. ) ;
#5589 = ORIENTED_EDGE ( 'NONE', *, *, #2060, .T. ) ;
#5590 = CARTESIAN_POINT ( 'NONE',  ( 1.030267906253071075, 0.6000000000000137446, 4.508336184329987617 ) ) ;
#5591 = EDGE_CURVE ( 'NONE', #5263, #16755, #11349, .T. ) ;
#5592 = VECTOR ( 'NONE', #18237, 1000.000000000000000 ) ;
#5593 = AXIS2_PLACEMENT_3D ( 'NONE', #4996, #15928, #17584 ) ;
#5594 = CARTESIAN_POINT ( 'NONE',  ( -3.333333333333390325, -2.694301256218301965, -3.300726591567088253 ) ) ;
#5595 = CARTESIAN_POINT ( 'NONE',  ( 66.26395429947837101, 0.000000000000000000, -5.999999999999908518 ) ) ;
#5596 = B_SPLINE_CURVE_WITH_KNOTS ( 'NONE', 3,
 ( #22229, #710, #2341, #21773, #4328 ),
 .UNSPECIFIED., .F., .F.,
 ( 4, 1, 4 ),
 ( 0.000000000000000000, 0.002020725942163693108, 0.004041451884327386217 ),
 .UNSPECIFIED. ) ;
#5597 = CARTESIAN_POINT ( 'NONE',  ( -12.84999999999999964, -12.50000000000011191, -5.749999999999936051 ) ) ;
#5598 = FACE_OUTER_BOUND ( 'NONE', #394, .T. ) ;
#5599 = CARTESIAN_POINT ( 'NONE',  ( -6.999999999708142795, 38.99999999900385461, -26.50000000000000000 ) ) ;
#5600 = DIRECTION ( 'NONE',  ( 0.000000000000000000, -1.734723475976805517E-15, 1.000000000000000000 ) ) ;
#5601 = SURFACE_SIDE_STYLE ('',( #23255 ) ) ;
#5602 = COLOUR_RGB ( '', 0.31764706, 0.68627451, 0.89019608) ;
#5603 = CARTESIAN_POINT ( 'NONE',  ( 119.5756419024615553, -4.000000000000003553, 6.000000000000136779 ) ) ;
#5604 = AXIS2_PLACEMENT_3D ( 'NONE', #9429, #2248, #9546 ) ;
#5605 = CARTESIAN_POINT ( 'NONE',  ( 37.86602540378474657, 11.00000000000000533, -2.133974596215531427 ) ) ;
#5606 = VERTEX_POINT ( 'NONE', #16704 ) ;
#5607 = TOROIDAL_SURFACE ( 'NONE', #22879, 5.500000000000003553, 0.5000000000000000000 ) ;
#5608 = AXIS2_PLACEMENT_3D ( 'NONE', #7360, #3476, #17836 ) ;
#5609 = CYLINDRICAL_SURFACE ( 'NONE', #8613, 2.500000000000002220 ) ;
#5611 = ORIENTED_EDGE ( 'NONE', *, *, #10211, .T. ) ;
#5610 = ORIENTED_EDGE ( 'NONE', *, *, #19725, .F. ) ;
#5612 = VERTEX_POINT ( 'NONE', #7556 ) ;
#5613 = ORIENTED_EDGE ( 'NONE', *, *, #3838, .T. ) ;
#5614 = ORIENTED_EDGE ( 'NONE', *, *, #15451, .F. ) ;
#5615 = ORIENTED_EDGE ( 'NONE', *, *, #8507, .T. ) ;
#5616 = EDGE_CURVE ( 'NONE', #10396, #14621, #14003, .T. ) ;
#5617 = DIRECTION ( 'NONE',  ( 0.000000000000000000, -1.000000000000000000, 0.000000000000000000 ) ) ;
#5618 = DIRECTION ( 'NONE',  ( 3.885780586188016830E-16, 4.437342591868156373E-31, -1.000000000000000000 ) ) ;
#5619 = DIRECTION ( 'NONE',  ( 0.7071067811865233699, -0.7071067811865715536, -1.565905175853783930E-16 ) ) ;
#5620 = CARTESIAN_POINT ( 'NONE',  ( -1.312671235360486133, -3.860931062424260762, -0.05923475698275939422 ) ) ;
#5621 = CARTESIAN_POINT ( 'NONE',  ( 3.973110223767125859, 2.263145622885971846E-11, 3.565797985667392922 ) ) ;
#5622 = CIRCLE ( 'NONE', #12745, 0.5000000000000004441 ) ;
#5623 = CARTESIAN_POINT ( 'NONE',  ( 8.113551354210024158, -12.41661007101923531, 7.426820295479682699 ) ) ;
#5624 = DIRECTION ( 'NONE',  ( -8.438582421954109416E-32, 0.000000000000000000, -1.000000000000000000 ) ) ;
#5625 = DIRECTION ( 'NONE',  ( 0.7313537016191733464, -0.6819983600624954789, 3.733258675956564523E-18 ) ) ;
#5626 = LINE ( 'NONE', #15840, #3311 ) ;
#5627 = AXIS2_PLACEMENT_3D ( 'NONE', #2885, #13043, #20667 ) ;
#5628 = CARTESIAN_POINT ( 'NONE',  ( 7.955953741309973459, -1.644172503818053688, 7.654083333123856470 ) ) ;
#5629 = CARTESIAN_POINT ( 'NONE',  ( 88.75737332930594903, -13.52760560296348302, 6.000000000000130562 ) ) ;
#5630 = CARTESIAN_POINT ( 'NONE',  ( 37.42127086598692642, 0.2176602893534504424, -10.42127086598688912 ) ) ;
#5631 = CARTESIAN_POINT ( 'NONE',  ( -3.673643420401913939, -2.497823135841291009, -0.2484800633750125221 ) ) ;
#5632 = DIRECTION ( 'NONE',  ( 1.000000000000000000, 2.220446049250313081E-16, -3.656342123407315983E-48 ) ) ;
#5633 = ORIENTED_EDGE ( 'NONE', *, *, #15869, .T. ) ;
#5634 = EDGE_CURVE ( 'NONE', #9332, #10367, #6025, .T. ) ;
#5635 = ORIENTED_EDGE ( 'NONE', *, *, #16023, .T. ) ;
#5636 = ADVANCED_FACE ( 'NONE', ( #20368 ), #863, .T. ) ;
#5637 = DIRECTION ( 'NONE',  ( -1.000000000000000000, 1.550910762415506096E-16, 0.000000000000000000 ) ) ;
#5638 = DIRECTION ( 'NONE',  ( -1.066786462891689527E-26, -6.656013887802287108E-31, -1.000000000000000000 ) ) ;
#5639 = VERTEX_POINT ( 'NONE', #6140 ) ;
#5640 = VECTOR ( 'NONE', #20288, 1000.000000000000000 ) ;
#5641 = CARTESIAN_POINT ( 'NONE',  ( -6.147973203409447862, 36.05667699661075432, -18.72569195403428566 ) ) ;
#5642 = DIRECTION ( 'NONE',  ( -1.000000000000000000, 1.276756478318923119E-15, -1.403805528459192781E-15 ) ) ;
#5643 = DIRECTION ( 'NONE',  ( -3.885780586188016830E-16, -4.437342591868156373E-31, 1.000000000000000000 ) ) ;
#5644 = LINE ( 'NONE', #12806, #21420 ) ;
#5646 = ORIENTED_EDGE ( 'NONE', *, *, #21775, .F. ) ;
#5645 = EDGE_CURVE ( 'NONE', #2907, #14077, #16233, .T. ) ;
#5647 = FACE_OUTER_BOUND ( 'NONE', #482, .T. ) ;
#5648 = DIRECTION ( 'NONE',  ( 0.000000000000000000, 0.000000000000000000, -1.000000000000000000 ) ) ;
#5649 = ADVANCED_FACE ( 'NONE', ( #17407 ), #9901, .T. ) ;
#5650 = B_SPLINE_CURVE_WITH_KNOTS ( 'NONE', 3,
 ( #20340, #16337, #21656, #21768 ),
 .UNSPECIFIED., .F., .F.,
 ( 4, 4 ),
 ( 0.000000000000000000, 1.361771040838494909E-05 ),
 .UNSPECIFIED. ) ;
#5651 = DIRECTION ( 'NONE',  ( 2.013525853219271912E-32, -5.941108692445745160E-30, -1.000000000000000000 ) ) ;
#5652 = EDGE_CURVE ( 'NONE', #919, #16755, #10234, .T. ) ;
#5653 = DIRECTION ( 'NONE',  ( 4.440892098500626162E-16, -1.000000000000000000, 1.263410043518026720E-31 ) ) ;
#5654 = CARTESIAN_POINT ( 'NONE',  ( 7.282868595548778856, -13.73825694947798937, 8.010178330700917115 ) ) ;
#5655 = CARTESIAN_POINT ( 'NONE',  ( -42.54314575050785407, -8.000000000000021316, 8.000000000000007105 ) ) ;
#5656 = DIRECTION ( 'NONE',  ( -0.1556420233463076119, 0.000000000000000000, -0.9878135252003121813 ) ) ;
#5657 = CARTESIAN_POINT ( 'NONE',  ( 85.68838070902455684, -9.818697260249752645, 6.500000000000158096 ) ) ;
#5658 = CARTESIAN_POINT ( 'NONE',  ( 37.00000000000017053, 0.2500000000000002220, -2.566987298107781257 ) ) ;
#5659 = CARTESIAN_POINT ( 'NONE',  ( 124.5000000000019469, -7.000000000000062172, 2.550000000000033573 ) ) ;
#5660 = AXIS2_PLACEMENT_3D ( 'NONE', #5794, #20132, #21793 ) ;
#5661 = EDGE_CURVE ( 'NONE', #6467, #15244, #19253, .T. ) ;
#5662 = DIRECTION ( 'NONE',  ( 9.693522803355793065E-26, -5.963788443470848352E-28, -1.000000000000000000 ) ) ;
#5663 = EDGE_CURVE ( 'NONE', #22523, #7574, #15412, .T. ) ;
#5664 = EDGE_CURVE ( 'NONE', #9669, #12565, #2840, .T. ) ;
#5665 = PRODUCT_CONTEXT ( 'NONE', #14753, 'mechanical' ) ;
#5666 = EDGE_LOOP ( 'NONE', ( #3550, #2113, #3921, #10997 ) ) ;
#5667 = ORIENTED_EDGE ( 'NONE', *, *, #5085, .F. ) ;
#5669 = ORIENTED_EDGE ( 'NONE', *, *, #586, .T. ) ;
#5668 = VERTEX_POINT ( 'NONE', #4827 ) ;
#5670 = ADVANCED_FACE ( 'NONE', ( #15530 ), #3072, .F. ) ;
#5671 = PLANE ( 'NONE',  #8418 ) ;
#5672 = CARTESIAN_POINT ( 'NONE',  ( 37.86602540378466841, -1.973247953923618070E-14, -2.133974596215482578 ) ) ;
#5673 = FACE_OUTER_BOUND ( 'NONE', #14310, .T. ) ;
#5674 = ADVANCED_FACE ( 'NONE', ( #11648 ), #6703, .T. ) ;
#5675 = AXIS2_PLACEMENT_3D ( 'NONE', #3068, #13772, #1534 ) ;
#5676 = CARTESIAN_POINT ( 'NONE',  ( -47.47487373415326317, 4.018019484660594109, -7.500000000000034639 ) ) ;
#5677 = CARTESIAN_POINT ( 'NONE',  ( 2.792295943733760366E-14, 11.99999999999999645, 2.500000000000000888 ) ) ;
#5678 = CARTESIAN_POINT ( 'NONE',  ( 4.114405500665259119, -2.025575754679715512, 3.508400121684935424 ) ) ;
#5679 = CARTESIAN_POINT ( 'NONE',  ( -6.917363703046245149, 36.00086243655339757, -18.25935642526717828 ) ) ;
#5680 =( NAMED_UNIT ( * ) SI_UNIT ( $, .STERADIAN. ) SOLID_ANGLE_UNIT ( ) );
#5681 = DIRECTION ( 'NONE',  ( -3.885780586188016830E-16, -4.437342591868156373E-31, 1.000000000000000000 ) ) ;
#5682 = CARTESIAN_POINT ( 'NONE',  ( 1.218648372641311897E-15, 59.74999999999991473, 4.500000000000020428 ) ) ;
#5683 = CARTESIAN_POINT ( 'NONE',  ( 4.197393957002244491, 7.205051708611501750E-14, -3.503767560748914711 ) ) ;
#5684 = CARTESIAN_POINT ( 'NONE',  ( 0.000000000000000000, 0.000000000000000000, -5.574599999999999334 ) ) ;
#5685 = DIRECTION ( 'NONE',  ( 1.000000000000000000, -4.440892098500654758E-16, 0.000000000000000000 ) ) ;
#5686 = CARTESIAN_POINT ( 'NONE',  ( 7.576750937466539604, -2.112750738699229469, 7.200086239788012321 ) ) ;
#5687 = DIRECTION ( 'NONE',  ( -1.733449886265891589E-32, 4.190823558986610327E-31, -1.000000000000000000 ) ) ;
#5688 = DIRECTION ( 'NONE',  ( 1.001543064812511222E-16, 2.634795423438190192E-27, -1.000000000000000000 ) ) ;
#5689 = VERTEX_POINT ( 'NONE', #8362 ) ;
#5690 =( NAMED_UNIT ( * ) SI_UNIT ( $, .STERADIAN. ) SOLID_ANGLE_UNIT ( ) );
#5691 = CIRCLE ( 'NONE', #10190, 0.5000000000000029976 ) ;
#5692 = CIRCLE ( 'NONE', #6812, 7.882182279042429407 ) ;
#5694 = ORIENTED_EDGE ( 'NONE', *, *, #21040, .F. ) ;
#5693 = ORIENTED_EDGE ( 'NONE', *, *, #519, .F. ) ;
#5695 = B_SPLINE_CURVE_WITH_KNOTS ( 'NONE', 3,
 ( #7490, #7039, #9027, #14211, #209, #21732 ),
 .UNSPECIFIED., .F., .F.,
 ( 4, 2, 4 ),
 ( 0.000000000000000000, 0.002086519881787257148, 0.004173039763574514296 ),
 .UNSPECIFIED. ) ;
#5696 = ORIENTED_EDGE ( 'NONE', *, *, #8398, .T. ) ;
#5697 = EDGE_LOOP ( 'NONE', ( #719, #12360 ) ) ;
#5699 = EDGE_LOOP ( 'NONE', ( #7457, #7370, #9568, #11366 ) ) ;
#5698 = VERTEX_POINT ( 'NONE', #22722 ) ;
#5700 = EDGE_LOOP ( 'NONE', ( #17127, #2973, #23154, #14138, #12358, #8466, #22562, #15427, #1103 ) ) ;
#5701 = EDGE_CURVE ( 'NONE', #17530, #4755, #16460, .T. ) ;
#5702 = DIRECTION ( 'NONE',  ( 0.000000000000000000, 0.000000000000000000, 1.000000000000000000 ) ) ;
#5703 = VERTEX_POINT ( 'NONE', #17173 ) ;
#5704 = ORIENTED_EDGE ( 'NONE', *, *, #20698, .T. ) ;
#5705 = DIRECTION ( 'NONE',  ( 0.000000000000000000, -0.5000000000000017764, 0.8660254037844375974 ) ) ;
#5706 = CARTESIAN_POINT ( 'NONE',  ( 4.211140560182194292, -2.431303136016568889, -3.745885042887441063 ) ) ;
#5707 = LINE ( 'NONE', #19940, #7161 ) ;
#5708 = EDGE_CURVE ( 'NONE', #9220, #6218, #1074, .T. ) ;
#5709 = CARTESIAN_POINT ( 'NONE',  ( 30.00000000029184832, 2.999999999003851503, -5.999999999999998224 ) ) ;
#5710 = CARTESIAN_POINT ( 'NONE',  ( 7.500000000000007105, -8.000000000000017764, 10.24999999999999467 ) ) ;
#5711 = CARTESIAN_POINT ( 'NONE',  ( -43.06238456605046849, 5.319238815542546739, -7.499999999999978684 ) ) ;
#5712 = AXIS2_PLACEMENT_3D ( 'NONE', #9960, #10297, #12047 ) ;
#5713 = CIRCLE ( 'NONE', #21503, 0.5000000000000004441 ) ;
#5714 = DIRECTION ( 'NONE',  ( 1.000000000000000000, -1.847414967615758933E-47, 3.885780586188017323E-16 ) ) ;
#5715 = DIRECTION ( 'NONE',  ( 1.000000000000000000, 2.699383410053119644E-30, 3.330669073875432643E-16 ) ) ;
#5716 = DIRECTION ( 'NONE',  ( -1.000000000000000000, 1.276756478318922922E-15, -1.333893503340766797E-15 ) ) ;
#5717 = ADVANCED_FACE ( 'NONE', ( #968 ), #20232, .T. ) ;
#5718 = CARTESIAN_POINT ( 'NONE',  ( 37.60054931026106573, 10.94797865062592024, -2.399450689738686027 ) ) ;
#5719 = ORIENTED_EDGE ( 'NONE', *, *, #1628, .F. ) ;
#5720 = DIRECTION ( 'NONE',  ( 3.885780586188016830E-16, 4.437342591868156373E-31, -1.000000000000000000 ) ) ;
#5722 = VERTEX_POINT ( 'NONE', #13777 ) ;
#5721 = ORIENTED_EDGE ( 'NONE', *, *, #15099, .T. ) ;
#5723 = ORIENTED_EDGE ( 'NONE', *, *, #11203, .T. ) ;
#5724 = EDGE_LOOP ( 'NONE', ( #13360, #17359, #6595, #17186, #21188, #1641, #4570, #11893, #11633, #18768, #10715, #13351 ) ) ;
#5725 = TOROIDAL_SURFACE ( 'NONE', #458, 4.500000000000000888, 0.5000000000000000000 ) ;
#5726 = AXIS2_PLACEMENT_3D ( 'NONE', #17134, #18804, #16669 ) ;
#5727 = ORIENTED_EDGE ( 'NONE', *, *, #22746, .T. ) ;
#5728 = CIRCLE ( 'NONE', #7650, 6.700000000000039257 ) ;
#5729 = ORIENTED_EDGE ( 'NONE', *, *, #4767, .T. ) ;
#5730 = CARTESIAN_POINT ( 'NONE',  ( -12.85000000000001386, 0.000000000000000000, -5.749999999999991118 ) ) ;
#5731 = CARTESIAN_POINT ( 'NONE',  ( -87.15000000000055991, -3.200000000000092104, -2.000000000000002220 ) ) ;
#5732 = CARTESIAN_POINT ( 'NONE',  ( 4.093692494532772841, -2.021783646005771207, -3.501831996793843604 ) ) ;
#5733 = VECTOR ( 'NONE', #23109, 1000.000000000000000 ) ;
#5734 = CARTESIAN_POINT ( 'NONE',  ( -9.714451465470119729E-14, -4.618802153517051146, -0.5000000000000004441 ) ) ;
#5735 = DIRECTION ( 'NONE',  ( 0.000000000000000000, 0.000000000000000000, 1.000000000000000000 ) ) ;
#5736 = CARTESIAN_POINT ( 'NONE',  ( 7.629227790279509591, -12.04719844907615744, 8.369856247450654152 ) ) ;
#5737 = CARTESIAN_POINT ( 'NONE',  ( 0.3126073911696378160, -2.020725942163709377, 3.500000000000003109 ) ) ;
#5738 = CARTESIAN_POINT ( 'NONE',  ( -7.491585531133505782, -2.143791077336254958, 7.320610673787135703 ) ) ;
#5739 = PLANE ( 'NONE',  #14207 ) ;
#5740 = CIRCLE ( 'NONE', #1240, 0.5000000000000029976 ) ;
#5741 = CARTESIAN_POINT ( 'NONE',  ( -3.674234614174765046, -0.7499999999999451550, -3.000000000000051070 ) ) ;
#5742 = DIRECTION ( 'NONE',  ( 1.000000000000000000, 3.254448077276381206E-32, 1.066788928082016908E-26 ) ) ;
#5743 = AXIS2_PLACEMENT_3D ( 'NONE', #17132, #20571, #1277 ) ;
#5744 = CARTESIAN_POINT ( 'NONE',  ( 2.918498775983380256E-10, -9.961476088449217059E-10, -45.00000000000000000 ) ) ;
#5745 = VECTOR ( 'NONE', #11128, 1000.000000000000000 ) ;
#5746 = EDGE_CURVE ( 'NONE', #21208, #22909, #2946, .T. ) ;
#5747 = AXIS2_PLACEMENT_3D ( 'NONE', #1499, #22917, #6789 ) ;
#5748 = CARTESIAN_POINT ( 'NONE',  ( 4.330127018922110160, 4.999999999999976907, -7.500000000000003553 ) ) ;
#5749 = DIRECTION ( 'NONE',  ( 0.000000000000000000, 0.000000000000000000, 1.000000000000000000 ) ) ;
#5750 = ORIENTED_EDGE ( 'NONE', *, *, #2789, .F. ) ;
#5751 = CYLINDRICAL_SURFACE ( 'NONE', #18513, 0.5000000000000025535 ) ;
#5752 = CARTESIAN_POINT ( 'NONE',  ( 84.32438398889952680, -11.28140466348809312, 6.500000000000137668 ) ) ;
#5753 = ORIENTED_EDGE ( 'NONE', *, *, #6708, .F. ) ;
#5754 = VECTOR ( 'NONE', #3776, 1000.000000000000000 ) ;
#5755 = DIRECTION ( 'NONE',  ( 1.000000000000000000, 3.254448077276381206E-32, 1.066788928082016908E-26 ) ) ;
#5756 = CIRCLE ( 'NONE', #21551, 6.000000000000036415 ) ;
#5757 = AXIS2_PLACEMENT_3D ( 'NONE', #15694, #22893, #3370 ) ;
#5758 = DIRECTION ( 'NONE',  ( -2.220446049250313081E-16, 1.000000000000000000, -7.025792437124636392E-31 ) ) ;
#5759 = CARTESIAN_POINT ( 'NONE',  ( 7.026577802269679651, -11.35109376985338869, 8.453373545151615431 ) ) ;
#5760 = CARTESIAN_POINT ( 'NONE',  ( -45.91923881554271958, -2.462384566050183743, -7.500000000000034639 ) ) ;
#5761 = CIRCLE ( 'NONE', #8758, 5.500000000000032863 ) ;
#5762 = CARTESIAN_POINT ( 'NONE',  ( -2.893953949542924385E-14, 4.736522675502212287, -3.681124513963636602 ) ) ;
#5763 = CARTESIAN_POINT ( 'NONE',  ( 12.84999999999998721, -12.50000000000011191, -6.249999999999936051 ) ) ;
#5764 = DIRECTION ( 'NONE',  ( -3.070652698126927723E-17, -1.000000000000000000, 4.167305704548413124E-17 ) ) ;
#5765 = FACE_OUTER_BOUND ( 'NONE', #4548, .T. ) ;
#5766 = DIRECTION ( 'NONE',  ( 3.885780586188016830E-16, 4.437342591868156373E-31, -1.000000000000000000 ) ) ;
#5767 = DIRECTION ( 'NONE',  ( 1.000000000000000000, -1.276756478318923119E-15, 1.342345546886807594E-15 ) ) ;
#5768 = DIRECTION ( 'NONE',  ( 3.885780586188016830E-16, 4.437342591868156373E-31, -1.000000000000000000 ) ) ;
#5769 = CARTESIAN_POINT ( 'NONE',  ( 4.052424581287912275, 2.393186648133639238, -2.990837702970695400 ) ) ;
#5770 = CARTESIAN_POINT ( 'NONE',  ( 1.369266385878517678, 0.000000000000000000, 0.000000000000000000 ) ) ;
#5771 = CARTESIAN_POINT ( 'NONE',  ( -3.999999999708153453, 35.99999999900384751, -26.50000000000000000 ) ) ;
#5772 = EDGE_CURVE ( 'NONE', #14225, #13530, #4589, .T. ) ;
#5773 = CIRCLE ( 'NONE', #13660, 0.4999999999999995559 ) ;
#5774 = CARTESIAN_POINT ( 'NONE',  ( 3.950241966888154099, -2.668221755853662724, -2.378504353000910676 ) ) ;
#5775 = CIRCLE ( 'NONE', #21564, 11.16066016895667268 ) ;
#5776 = TOROIDAL_SURFACE ( 'NONE', #20417, 4.366025403784441039, 0.5000000000000000000 ) ;
#5777 = AXIS2_PLACEMENT_3D ( 'NONE', #5563, #3779, #261 ) ;
#5778 = CIRCLE ( 'NONE', #10282, 9.500000000000056843 ) ;
#5779 = AXIS2_PLACEMENT_3D ( 'NONE', #11638, #16924, #2700 ) ;
#5780 = ADVANCED_FACE ( 'NONE', ( #8254 ), #22104, .T. ) ;
#5781 = SHAPE_DEFINITION_REPRESENTATION ( #13619, #4439 ) ;
#5782 = EDGE_CURVE ( 'NONE', #6059, #9570, #22475, .T. ) ;
#5783 = ORIENTED_EDGE ( 'NONE', *, *, #13872, .F. ) ;
#5784 = EDGE_CURVE ( 'NONE', #10359, #22613, #2566, .T. ) ;
#5786 = ORIENTED_EDGE ( 'NONE', *, *, #2102, .T. ) ;
#5785 = ORIENTED_EDGE ( 'NONE', *, *, #22142, .F. ) ;
#5787 = PLANE ( 'NONE',  #9904 ) ;
#5788 = CARTESIAN_POINT ( 'NONE',  ( 37.22062532321634620, 0.1155932590976544300, -2.456674636499718289 ) ) ;
#5789 = AXIS2_PLACEMENT_3D ( 'NONE', #11138, #331, #16763 ) ;
#5790 =( BOUNDED_CURVE ( )  B_SPLINE_CURVE ( 3, ( #17887, #1536, #19408, #18008 ),
 .UNSPECIFIED., .F., .T. ) 
 B_SPLINE_CURVE_WITH_KNOTS ( ( 4, 4 ),
 ( 3.665191429188060734, 4.712388980384689674 ),
 .UNSPECIFIED. ) 
 CURVE ( )  GEOMETRIC_REPRESENTATION_ITEM ( )  RATIONAL_B_SPLINE_CURVE ( ( 1.000000000000000000, 0.9106836025229538834, 0.9106836025229538834, 1.000000000000000000 ) ) 
 REPRESENTATION_ITEM ( '' )  );
#5791 = ORIENTED_EDGE ( 'NONE', *, *, #6119, .F. ) ;
#5792 = VECTOR ( 'NONE', #10731, 1000.000000000000000 ) ;
#5793 = CARTESIAN_POINT ( 'NONE',  ( -5.484827557301438894, 1.325747111984031834, 0.000000000000000000 ) ) ;
#5794 = CARTESIAN_POINT ( 'NONE',  ( 22.49999999999999645, 4.250000000000031974, -1.249999999999997558 ) ) ;
#5795 = AXIS2_PLACEMENT_3D ( 'NONE', #11725, #9856, #9747 ) ;
#5796 = CARTESIAN_POINT ( 'NONE',  ( -45.37157287525410254, 6.828427124746169419, 8.000000000000035527 ) ) ;
#5798 = EDGE_CURVE ( 'NONE', #19780, #6327, #4063, .T. ) ;
#5797 = CARTESIAN_POINT ( 'NONE',  ( -4.211140560182312420, 2.431303136016568889, -3.745885042887433958 ) ) ;
#5799 = EDGE_CURVE ( 'NONE', #6309, #17226, #12464, .T. ) ;
#5800 = FACE_OUTER_BOUND ( 'NONE', #6910, .T. ) ;
#5801 = DIRECTION ( 'NONE',  ( -0.7313537016191745677, -0.6819983600624940356, -1.072890437865584285E-16 ) ) ;
#5802 = DIRECTION ( 'NONE',  ( 1.733449886265891589E-32, -4.190823558986610327E-31, 1.000000000000000000 ) ) ;
#5803 = CARTESIAN_POINT ( 'NONE',  ( 0.000000000000000000, 0.000000000000000000, 0.000000000000000000 ) ) ;
#5804 =( REPRESENTATION_RELATIONSHIP ('NONE','NONE', #19450, #20536 ) REPRESENTATION_RELATIONSHIP_WITH_TRANSFORMATION ( #14932 )SHAPE_REPRESENTATION_RELATIONSHIP( ) );
#5805 =( NAMED_UNIT ( * ) PLANE_ANGLE_UNIT ( ) SI_UNIT ( $, .RADIAN. ) );
#5806 = DIRECTION ( 'NONE',  ( 0.000000000000000000, 0.000000000000000000, -1.000000000000000000 ) ) ;
#5807 = ADVANCED_FACE ( 'NONE', ( #7310 ), #10479, .T. ) ;
#5808 = CARTESIAN_POINT ( 'NONE',  ( 4.050823680195218657, -3.779313952391380571, 0.5899027668435161686 ) ) ;
#5809 = DIRECTION ( 'NONE',  ( 9.121204216617949000E-31, 1.000000000000000000, -6.982962677686261977E-15 ) ) ;
#5810 = DIRECTION ( 'NONE',  ( 1.066786462891689527E-26, 6.656013887802287108E-31, 1.000000000000000000 ) ) ;
#5811 = CARTESIAN_POINT ( 'NONE',  ( 5.775087817974630717E-16, 3.375361811986508975, -1.153701847711636086 ) ) ;
#5812 = ORIENTED_EDGE ( 'NONE', *, *, #19181, .T. ) ;
#5813 = AXIS2_PLACEMENT_3D ( 'NONE', #6402, #1340, #8281 ) ;
#5814 = ADVANCED_FACE ( 'NONE', ( #19651 ), #8836, .T. ) ;
#5815 = CIRCLE ( 'NONE', #2418, 9.500000000000063949 ) ;
#5817 = VERTEX_POINT ( 'NONE', #6964 ) ;
#5816 = ORIENTED_EDGE ( 'NONE', *, *, #15133, .T. ) ;
#5818 = UNCERTAINTY_MEASURE_WITH_UNIT (LENGTH_MEASURE( 1.000000000000000082E-05 ), #4146, 'distance_accuracy_value', 'NONE');
#5819 = CIRCLE ( 'NONE', #13681, 4.750000000000000000 ) ;
#5820 = ADVANCED_FACE ( 'NONE', ( #3543 ), #14955, .F. ) ;
#5821 = ORIENTED_EDGE ( 'NONE', *, *, #16114, .T. ) ;
#5822 = ORIENTED_EDGE ( 'NONE', *, *, #597, .F. ) ;
#5824 = ORIENTED_EDGE ( 'NONE', *, *, #8630, .T. ) ;
#5823 = ORIENTED_EDGE ( 'NONE', *, *, #22327, .F. ) ;
#5825 = VERTEX_POINT ( 'NONE', #14244 ) ;
#5826 = CARTESIAN_POINT ( 'NONE',  ( 12.84999999999997300, -0.5000000000000004441, 1.387778780781445676E-14 ) ) ;
#5827 = EDGE_LOOP ( 'NONE', ( #7002, #15717, #1934, #10316 ) ) ;
#5828 = ORIENTED_EDGE ( 'NONE', *, *, #10930, .F. ) ;
#5829 = CARTESIAN_POINT ( 'NONE',  ( 4.000000000000003553, 1.557668341133516599, -0.1596965656957576030 ) ) ;
#5830 = CARTESIAN_POINT ( 'NONE',  ( 2.085593006335303400E-14, -3.273442688548351087E-16, -2.500000000000000000 ) ) ;
#5831 = EDGE_CURVE ( 'NONE', #3520, #14012, #19887, .T. ) ;
#5832 = CARTESIAN_POINT ( 'NONE',  ( -7.161440864725758360, -2.387752514309356311, 7.973376427817367329 ) ) ;
#5833 = EDGE_CURVE ( 'NONE', #9593, #18558, #15711, .T. ) ;
#5834 = ADVANCED_BREP_SHAPE_REPRESENTATION ( '', ( #21055, #22115 ), #7475 ) ;
#5835 = FACE_OUTER_BOUND ( 'NONE', #599, .T. ) ;
#5836 = AXIS2_PLACEMENT_3D ( 'NONE', #12476, #19669, #21674 ) ;
#5837 = CARTESIAN_POINT ( 'NONE',  ( 63.53596085922831804, -2.925414806476678287, 6.000000000000136779 ) ) ;
#5838 = CARTESIAN_POINT ( 'NONE',  ( 0.000000000000000000, 0.000000000000000000, 0.000000000000000000 ) ) ;
#5839 = FACE_OUTER_BOUND ( 'NONE', #13270, .T. ) ;
#5840 = DIRECTION ( 'NONE',  ( 2.775557561562883955E-17, -3.406761633869148826E-16, 1.000000000000000000 ) ) ;
#5841 = EDGE_CURVE ( 'NONE', #22552, #6184, #17599, .T. ) ;
#5842 = CARTESIAN_POINT ( 'NONE',  ( 37.48161866288229760, 10.82270004028423571, -2.902788078020195339 ) ) ;
#5843 = ORIENTED_EDGE ( 'NONE', *, *, #17863, .F. ) ;
#5844 = UNCERTAINTY_MEASURE_WITH_UNIT (LENGTH_MEASURE( 1.000000000000000082E-05 ), #18615, 'distance_accuracy_value', 'NONE');
#5845 = DIRECTION ( 'NONE',  ( -1.000000000000000000, 0.000000000000000000, -1.613696256722611405E-16 ) ) ;
#5847 = ORIENTED_EDGE ( 'NONE', *, *, #10877, .T. ) ;
#5846 = ORIENTED_EDGE ( 'NONE', *, *, #17002, .T. ) ;
#5848 = ORIENTED_EDGE ( 'NONE', *, *, #5015, .T. ) ;
#5849 = ORIENTED_EDGE ( 'NONE', *, *, #17867, .T. ) ;
#5850 = ORIENTED_EDGE ( 'NONE', *, *, #915, .T. ) ;
#5851 = EDGE_LOOP ( 'NONE', ( #9186, #13745, #21418, #10932 ) ) ;
#5852 = CARTESIAN_POINT ( 'NONE',  ( -53.99613665484950786, 1.387778780781445676E-14, -13.19342998475048212 ) ) ;
#5853 = LINE ( 'NONE', #13017, #11358 ) ;
#5854 = CARTESIAN_POINT ( 'NONE',  ( 6.500000000000005329, 0.5000000000001669775, 3.469446951953614189E-14 ) ) ;
#5855 = CARTESIAN_POINT ( 'NONE',  ( 2.499999999999992006, 2.000000000000001776, -0.2500000000000349165 ) ) ;
#5856 = DIRECTION ( 'NONE',  ( 2.220446049250313081E-16, -1.000000000000000000, 7.025792437124636392E-31 ) ) ;
#5857 = CARTESIAN_POINT ( 'NONE',  ( -90.63385214007844581, 0.5000000000000490719, -7.926881151201908615 ) ) ;
#5858 = FACE_OUTER_BOUND ( 'NONE', #9976, .T. ) ;
#5859 = CARTESIAN_POINT ( 'NONE',  ( 12.84999999999997300, -2.011595308313580664E-30, 2.550000000000010925 ) ) ;
#5860 = CARTESIAN_POINT ( 'NONE',  ( -12.85000000000001386, -1.999999999999998224, -6.249999999999992006 ) ) ;
#5861 = CARTESIAN_POINT ( 'NONE',  ( -12.85000000000002807, -12.00000000000002842, 6.250000000000019540 ) ) ;
#5862 = EDGE_CURVE ( 'NONE', #19457, #1155, #18720, .T. ) ;
#5863 = DIRECTION ( 'NONE',  ( 1.000000000000000000, 0.000000000000000000, 0.000000000000000000 ) ) ;
#5864 = CIRCLE ( 'NONE', #19007, 0.5000000000000005551 ) ;
#5865 = CARTESIAN_POINT ( 'NONE',  ( -3.344563996438217224, -2.687817229851500400, -0.1586754815285019160 ) ) ;
#5866 = DIRECTION ( 'NONE',  ( 1.000000000000000000, 1.479114197289387852E-30, -2.013525853228518840E-32 ) ) ;
#5867 = ADVANCED_FACE ( 'NONE', ( #7191 ), #21401, .F. ) ;
#5868 = VERTEX_POINT ( 'NONE', #16216 ) ;
#5869 = DIRECTION ( 'NONE',  ( -9.121204216617949000E-31, -1.000000000000000000, 6.982962677686261977E-15 ) ) ;
#5870 = CARTESIAN_POINT ( 'NONE',  ( 6.500000000000088818, -13.52760560296348302, 6.500000000000075495 ) ) ;
#5871 = ORIENTED_EDGE ( 'NONE', *, *, #16998, .F. ) ;
#5872 = DIRECTION ( 'NONE',  ( 3.885780586188016830E-16, 4.437342591868156373E-31, -1.000000000000000000 ) ) ;
#5873 = DIRECTION ( 'NONE',  ( -1.000000000000000000, 1.276756478318922725E-15, -1.333893503340766402E-15 ) ) ;
#5874 = DIRECTION ( 'NONE',  ( 3.885780586188016830E-16, 4.437342591868156373E-31, -1.000000000000000000 ) ) ;
#5875 = DIRECTION ( 'NONE',  ( -2.220446049250313081E-16, 1.000000000000000000, -7.025792437124636392E-31 ) ) ;
#5876 = DIRECTION ( 'NONE',  ( -1.000000000000000000, 1.550910762415518915E-16, 0.000000000000000000 ) ) ;
#5877 = CARTESIAN_POINT ( 'NONE',  ( -4.499999999708154341, 35.49999999900384751, -26.00000000000000000 ) ) ;
#5878 = PLANE ( 'NONE',  #12058 ) ;
#5879 = DIRECTION ( 'NONE',  ( 1.000000000000000000, 0.000000000000000000, 0.000000000000000000 ) ) ;
#5880 = CIRCLE ( 'NONE', #603, 2.550000000000003819 ) ;
#5881 = CARTESIAN_POINT ( 'NONE',  ( 7.568268608011931242, -13.53268520232752614, 8.579161250779895553 ) ) ;
#5882 = CARTESIAN_POINT ( 'NONE',  ( -45.56568542494955665, 2.108831175456925333, -7.500000000000007105 ) ) ;
#5883 = ORIENTED_EDGE ( 'NONE', *, *, #14900, .F. ) ;
#5884 = DIRECTION ( 'NONE',  ( 0.9878135252003128475, 2.193386639427060968E-16, -0.1556420233463030045 ) ) ;
#5885 = FACE_OUTER_BOUND ( 'NONE', #14283, .T. ) ;
#5886 = CARTESIAN_POINT ( 'NONE',  ( -7.000000000000006217, 2.775557561562891351E-14, 12.24999999999996980 ) ) ;
#5887 = PLANE ( 'NONE',  #8957 ) ;
#5888 = ORIENTED_EDGE ( 'NONE', *, *, #1966, .F. ) ;
#5889 = CIRCLE ( 'NONE', #10755, 0.5000000000000028866 ) ;
#5891 = VERTEX_POINT ( 'NONE', #23083 ) ;
#5890 = ORIENTED_EDGE ( 'NONE', *, *, #18762, .T. ) ;
#5892 = DIRECTION ( 'NONE',  ( -1.000000000000000000, 1.813574543066650990E-15, 0.000000000000000000 ) ) ;
#5893 = CARTESIAN_POINT ( 'NONE',  ( 7.168696526429609861, -0.3737769141893478864, 8.340670630249134021 ) ) ;
#5894 = ADVANCED_FACE ( 'NONE', ( #21311 ), #131, .F. ) ;
#5895 = CARTESIAN_POINT ( 'NONE',  ( 36.00000000029184832, 2.999999999003851503, -26.50000000000000000 ) ) ;
#5896 = ORIENTED_EDGE ( 'NONE', *, *, #11876, .F. ) ;
#5897 = FACE_OUTER_BOUND ( 'NONE', #20595, .T. ) ;
#5898 = FACE_OUTER_BOUND ( 'NONE', #20449, .T. ) ;
#5899 = CARTESIAN_POINT ( 'NONE',  ( 1.199999999999992628, 0.000000000000000000, 0.000000000000000000 ) ) ;
#5900 = CARTESIAN_POINT ( 'NONE',  ( 116.8476484622116232, -8.074585193523331483, 6.000000000000136779 ) ) ;
#5901 = CYLINDRICAL_SURFACE ( 'NONE', #14059, 6.500000000000067502 ) ;
#5902 = AXIS2_PLACEMENT_3D ( 'NONE', #6618, #6508, #10495 ) ;
#5903 = CARTESIAN_POINT ( 'NONE',  ( 37.00000000000011369, 11.00000000000000000, -10.00000000000000888 ) ) ;
#5904 = DIRECTION ( 'NONE',  ( 1.000000000000000000, 1.479114197289397135E-31, 5.916456789157588541E-31 ) ) ;
#5905 = CARTESIAN_POINT ( 'NONE',  ( 4.000000000000003553, 2.309401076758480720, -5.600000000000000533 ) ) ;
#5906 = VECTOR ( 'NONE', #6749, 1000.000000000000000 ) ;
#5907 = DIRECTION ( 'NONE',  ( -7.860214984770699307E-18, 1.409037165336591006E-16, 1.000000000000000000 ) ) ;
#5908 = STYLED_ITEM ( 'NONE', ( #11302 ), #20836 ) ;
#5909 = CARTESIAN_POINT ( 'NONE',  ( -12.85000000000001386, -12.00000000000005151, 2.550000000000038902 ) ) ;
#5910 = DIRECTION ( 'NONE',  ( 9.693522803355793065E-26, -5.963788443470848352E-28, -1.000000000000000000 ) ) ;
#5911 = CARTESIAN_POINT ( 'NONE',  ( 8.233775472210654200, -0.5437072270125227202, 7.279685395985851848 ) ) ;
#5912 = ORIENTED_EDGE ( 'NONE', *, *, #20442, .T. ) ;
#5913 = AXIS2_PLACEMENT_3D ( 'NONE', #17379, #13638, #20830 ) ;
#5914 = SURFACE_SIDE_STYLE ('',( #22026 ) ) ;
#5916 = ORIENTED_EDGE ( 'NONE', *, *, #21499, .T. ) ;
#5915 = ORIENTED_EDGE ( 'NONE', *, *, #7261, .T. ) ;
#5917 = EDGE_LOOP ( 'NONE', ( #19977, #16108, #13089, #7233 ) ) ;
#5918 = EDGE_CURVE ( 'NONE', #15879, #16689, #12504, .T. ) ;
#5919 = ORIENTED_EDGE ( 'NONE', *, *, #9519, .F. ) ;
#5921 = VERTEX_POINT ( 'NONE', #10589 ) ;
#5920 = ORIENTED_EDGE ( 'NONE', *, *, #1496, .F. ) ;
#5922 = AXIS2_PLACEMENT_3D ( 'NONE', #3868, #21659, #7413 ) ;
#5923 = ORIENTED_EDGE ( 'NONE', *, *, #6250, .T. ) ;
#5924 = DIRECTION ( 'NONE',  ( 4.190823558986625216E-31, -1.000000000000000000, 4.190823558986625216E-31 ) ) ;
#5925 = AXIS2_PLACEMENT_3D ( 'NONE', #7028, #17959, #22907 ) ;
#5926 = ORIENTED_EDGE ( 'NONE', *, *, #12130, .T. ) ;
#5927 = EDGE_CURVE ( 'NONE', #18277, #18843, #18461, .T. ) ;
#5928 = ORIENTED_EDGE ( 'NONE', *, *, #17152, .F. ) ;
#5929 = CARTESIAN_POINT ( 'NONE',  ( -95.70000000000069917, 2.775557561562891351E-14, -2.000000000000001776 ) ) ;
#5930 = CARTESIAN_POINT ( 'NONE',  ( 0.02993401039714900166, -3.373851915354638020, -1.156317065392238774 ) ) ;
#5931 = LINE ( 'NONE', #8353, #4636 ) ;
#5932 = AXIS2_PLACEMENT_3D ( 'NONE', #3980, #2567, #4097 ) ;
#5933 = DIRECTION ( 'NONE',  ( -1.000000000000000000, -1.110223024625164429E-16, 1.298062744027674633E-32 ) ) ;
#5934 = DIRECTION ( 'NONE',  ( 0.000000000000000000, 3.382522293539642681E-32, 1.000000000000000000 ) ) ;
#5935 = CIRCLE ( 'NONE', #8552, 4.500000000000052403 ) ;
#5936 = EDGE_CURVE ( 'NONE', #15879, #13703, #7415, .T. ) ;
#5937 = CARTESIAN_POINT ( 'NONE',  ( 4.124214193018073793, -2.028338413290998510, -3.513185186763549961 ) ) ;
#5938 = DIRECTION ( 'NONE',  ( 1.000000000000000000, 2.220446049250313081E-16, 0.000000000000000000 ) ) ;
#5939 = EDGE_CURVE ( 'NONE', #3915, #13552, #21367, .T. ) ;
#5940 = CARTESIAN_POINT ( 'NONE',  ( 24.99999999999995737, 2.000000000000001776, -17.74999999999998224 ) ) ;
#5941 = B_SPLINE_CURVE_WITH_KNOTS ( 'NONE', 3,
 ( #14265, #3334, #15893, #157, #1680, #22978, #19678, #10842, #7106, #21454 ),
 .UNSPECIFIED., .F., .F.,
 ( 4, 2, 2, 2, 4 ),
 ( 0.003632676470446334280, 0.004026789025884817963, 0.004420901581323301646, 0.004815014136761786197, 0.005209126692200269880 ),
 .UNSPECIFIED. ) ;
#5942 = CYLINDRICAL_SURFACE ( 'NONE', #1575, 10.00000000000006395 ) ;
#5944 = EDGE_CURVE ( 'NONE', #21618, #23117, #16681, .T. ) ;
#5943 = CIRCLE ( 'NONE', #15674, 0.5000000000000038858 ) ;
#5945 = LINE ( 'NONE', #14645, #1063 ) ;
#5946 = DIRECTION ( 'NONE',  ( 0.000000000000000000, 0.000000000000000000, -1.000000000000000000 ) ) ;
#5947 = CIRCLE ( 'NONE', #5188, 2.549999999999997158 ) ;
#5948 = ORIENTED_EDGE ( 'NONE', *, *, #19313, .F. ) ;
#5949 = FACE_OUTER_BOUND ( 'NONE', #18306, .T. ) ;
#5951 = EDGE_LOOP ( 'NONE', ( #8577, #1635, #3153, #489 ) ) ;
#5950 = EDGE_LOOP ( 'NONE', ( #2383, #7232 ) ) ;
#5952 = AXIS2_PLACEMENT_3D ( 'NONE', #20695, #2810, #9987 ) ;
#5953 = EDGE_CURVE ( 'NONE', #7570, #22556, #3696, .T. ) ;
#5954 = EDGE_CURVE ( 'NONE', #22529, #2822, #16912, .T. ) ;
#5955 = VECTOR ( 'NONE', #15870, 1000.000000000000000 ) ;
#5956 = ADVANCED_FACE ( 'NONE', ( #21998 ), #16789, .F. ) ;
#5957 = ORIENTED_EDGE ( 'NONE', *, *, #21358, .T. ) ;
#5958 = VECTOR ( 'NONE', #20473, 1000.000000000000000 ) ;
#5959 = VERTEX_POINT ( 'NONE', #4210 ) ;
#5960 = ORIENTED_EDGE ( 'NONE', *, *, #23080, .F. ) ;
#5961 = DIRECTION ( 'NONE',  ( -2.172745813409349776E-17, 1.000000000000000000, -1.309377075419428048E-16 ) ) ;
#5962 = CARTESIAN_POINT ( 'NONE',  ( -12.85000000000001386, -14.00000000000008882, -2.549999999999945199 ) ) ;
#5963 = ADVANCED_FACE ( 'NONE', ( #5885 ), #11581, .T. ) ;
#5964 = ORIENTED_EDGE ( 'NONE', *, *, #22734, .F. ) ;
#5965 =( GEOMETRIC_REPRESENTATION_CONTEXT ( 3 ) GLOBAL_UNCERTAINTY_ASSIGNED_CONTEXT ( ( #12621 ) ) GLOBAL_UNIT_ASSIGNED_CONTEXT ( ( #22203, #16107, #11142 ) ) REPRESENTATION_CONTEXT ( 'NONE', 'WORKASPACE' ) );
#5966 = PLANE ( 'NONE',  #21121 ) ;
#5967 = EDGE_CURVE ( 'NONE', #5722, #16629, #11051, .T. ) ;
#5968 = CARTESIAN_POINT ( 'NONE',  ( 111.3116192909783848, -9.818697260249948044, -6.000000000000067502 ) ) ;
#5969 = DIRECTION ( 'NONE',  ( 0.000000000000000000, 0.000000000000000000, 1.000000000000000000 ) ) ;
#5970 = DIRECTION ( 'NONE',  ( 1.066786462891689527E-26, 6.656013887802287108E-31, 1.000000000000000000 ) ) ;
#5971 = CARTESIAN_POINT ( 'NONE',  ( 4.165266963751727225, 4.099263933823985795, -1.987707336973076212E-15 ) ) ;
#5972 =( BOUNDED_SURFACE ( )  B_SPLINE_SURFACE ( 3, 2, ( 
 ( #21058, #4919, #12327 ),
 ( #12085, #5, #12571 ),
 ( #21417, #21178, #10460 ),
 ( #15850, #19278, #5047 ),
 ( #12206, #3525, #23061 ),
 ( #5286, #10689, #14104 ),
 ( #5166, #19517, #12446 ),
 ( #10570, #17873, #8932 ) ),
 .UNSPECIFIED., .F., .F., .F. ) 
 B_SPLINE_SURFACE_WITH_KNOTS ( ( 4, 2, 2, 4 ),
 ( 3, 3 ),
 ( 0.000000000000000000, 0.0006647103312144571167, 0.001329420662428914233, 0.002658841324857828467 ),
 ( 0.000000000000000000, 1.000000000000000000 ),
 .UNSPECIFIED. ) 
 GEOMETRIC_REPRESENTATION_ITEM ( )  RATIONAL_B_SPLINE_SURFACE ( (
 ( 1.000000000000000000, 0.7071067811865475727, 1.000000000000000000),
 ( 1.000000000000000000, 0.7467694970713046887, 1.000000000000000000),
 ( 1.000000000000000000, 0.7847899295822856613, 1.000000000000000000),
 ( 1.000000000000000000, 0.8553546080387325334, 1.000000000000000000),
 ( 1.000000000000000000, 0.8874277420052644194, 1.000000000000000000),
 ( 1.000000000000000000, 0.9672515829027974466, 1.000000000000000000),
 ( 1.000000000000000000, 0.9993132011596692621, 1.000000000000000000),
 ( 1.000000000000000000, 0.9999716904335731460, 1.000000000000000000) ) ) 
 REPRESENTATION_ITEM ( '' )  SURFACE ( )  );
#5973 = LINE ( 'NONE', #11253, #2298 ) ;
#5974 = AXIS2_PLACEMENT_3D ( 'NONE', #2549, #16425, #16766 ) ;
#5975 = CYLINDRICAL_SURFACE ( 'NONE', #10845, 0.5000000000000038858 ) ;
#5976 = VECTOR ( 'NONE', #3371, 1000.000000000000000 ) ;
#5977 = DIRECTION ( 'NONE',  ( -1.000000000000000000, -1.910522504832140594E-31, 5.551115123125818447E-17 ) ) ;
#5978 = FACE_OUTER_BOUND ( 'NONE', #23119, .T. ) ;
#5979 = CARTESIAN_POINT ( 'NONE',  ( -4.000000000000003553, -2.309401076758532678, -0.3572655899081733644 ) ) ;
#5980 = CARTESIAN_POINT ( 'NONE',  ( 2.775557561562891351E-14, 11.99999999999999645, 6.938893903907228378E-15 ) ) ;
#5981 = ORIENTED_EDGE ( 'NONE', *, *, #6239, .T. ) ;
#5982 = EDGE_LOOP ( 'NONE', ( #8056, #23209, #20708, #18839, #3694, #10773, #7937 ) ) ;
#5983 = VERTEX_POINT ( 'NONE', #11506 ) ;
#5984 = DIRECTION ( 'NONE',  ( -9.693457064947022734E-26, 0.000000000000000000, 1.000000000000000000 ) ) ;
#5985 = AXIS2_PLACEMENT_3D ( 'NONE', #18523, #12767, #7708 ) ;
#5986 = DIRECTION ( 'NONE',  ( 1.000000000000000000, -1.424116703980815236E-16, -2.931272055834072749E-32 ) ) ;
#5987 = EDGE_LOOP ( 'NONE', ( #7706, #8026, #19573, #1832 ) ) ;
#5988 = VECTOR ( 'NONE', #19020, 1000.000000000000000 ) ;
#5989 = CIRCLE ( 'NONE', #19126, 0.5000000000000004441 ) ;
#5990 = CARTESIAN_POINT ( 'NONE',  ( 5.599999999999994316, 0.000000000000000000, 0.000000000000000000 ) ) ;
#5991 = EDGE_CURVE ( 'NONE', #16286, #13739, #18583, .T. ) ;
#5992 = DIRECTION ( 'NONE',  ( 1.454462294001240516E-30, 1.000000000000000000, 0.000000000000000000 ) ) ;
#5993 = FACE_OUTER_BOUND ( 'NONE', #13842, .T. ) ;
#5994 = DIRECTION ( 'NONE',  ( 1.734723475976813750E-16, 1.000000000000000000, -3.469446951953607484E-15 ) ) ;
#5995 = CARTESIAN_POINT ( 'NONE',  ( -42.54314575050793934, 3.999999999999996447, 7.500000000000062172 ) ) ;
#5996 = FACE_OUTER_BOUND ( 'NONE', #2375, .T. ) ;
#5997 = CARTESIAN_POINT ( 'NONE',  ( 4.560724896783636240, 0.7500000000000559552, -2.506869887779819450 ) ) ;
#5998 = ADVANCED_FACE ( 'NONE', ( #362 ), #9636, .F. ) ;
#5999 = DIRECTION ( 'NONE',  ( -1.000000000000000000, 7.477632011778292156E-48, -3.885780586188017323E-16 ) ) ;
#6000 = PRESENTATION_LAYER_ASSIGNMENT (  '', '', ( #22518 ) ) ;
#6001 = CARTESIAN_POINT ( 'NONE',  ( 7.756475484083226846, -13.93440482874969533, 7.145789564688786122 ) ) ;
#6002 = DIRECTION ( 'NONE',  ( 5.551115123561405253E-17, 1.000000000000000000, -5.963788443470795439E-28 ) ) ;
#6003 = CARTESIAN_POINT ( 'NONE',  ( -42.54314575050796776, 4.800000000000033573, -8.000000000000035527 ) ) ;
#6004 = CARTESIAN_POINT ( 'NONE',  ( 2.775557561562891351E-14, 0.000000000000000000, -6.499999999999950262 ) ) ;
#6005 = DIRECTION ( 'NONE',  ( 1.333893503340774882E-15, 2.778352770573747380E-17, 1.000000000000000000 ) ) ;
#6006 = CARTESIAN_POINT ( 'NONE',  ( 24.75000000000001066, 2.000000000000099032, -16.99999999999997868 ) ) ;
#6007 = ITEM_DEFINED_TRANSFORMATION ( 'NONE', 'NONE', #6010,  #22115 ) ;
#6008 = AXIS2_PLACEMENT_3D ( 'NONE', #7744, #14804, #20894 ) ;
#6009 = EDGE_LOOP ( 'NONE', ( #8546, #17361, #10622, #15816, #18818, #21030 ) ) ;
#6010 = AXIS2_PLACEMENT_3D ( 'NONE', #10140, #8374, #17296 ) ;
#6012 = ORIENTED_EDGE ( 'NONE', *, *, #20906, .F. ) ;
#6011 = ORIENTED_EDGE ( 'NONE', *, *, #6078, .T. ) ;
#6013 = DIRECTION ( 'NONE',  ( -2.013525853228508439E-32, -6.779273404243028164E-31, 1.000000000000000000 ) ) ;
#6014 = CARTESIAN_POINT ( 'NONE',  ( -50.65685424949270299, 7.200000000000025935, 7.500000000000062172 ) ) ;
#6015 =( NAMED_UNIT ( * ) PLANE_ANGLE_UNIT ( ) SI_UNIT ( $, .RADIAN. ) );
#6016 = ORIENTED_EDGE ( 'NONE', *, *, #12772, .T. ) ;
#6017 = CARTESIAN_POINT ( 'NONE',  ( -3.805981007006675298, -0.7499999999999436007, -3.000000000000016875 ) ) ;
#6018 = CYLINDRICAL_SURFACE ( 'NONE', #16538, 0.5000000000000038858 ) ;
#6019 = CYLINDRICAL_SURFACE ( 'NONE', #11375, 4.000000000000045297 ) ;
#6020 = CARTESIAN_POINT ( 'NONE',  ( 0.4425134659200216647, -0.5999999999999892086, 4.147378741782005385 ) ) ;
#6021 = CARTESIAN_POINT ( 'NONE',  ( -2.000000000000015543, 3.464101615137746837, -5.600000000000000533 ) ) ;
#6022 = CYLINDRICAL_SURFACE ( 'NONE', #10592, 0.5000000000000004441 ) ;
#6023 = AXIS2_PLACEMENT_3D ( 'NONE', #21987, #5875, #20229 ) ;
#6024 = CARTESIAN_POINT ( 'NONE',  ( -50.65685424949277404, -1.040834085586084257E-13, -7.500000000000062172 ) ) ;
#6025 = LINE ( 'NONE', #9436, #10988 ) ;
#6026 = CARTESIAN_POINT ( 'NONE',  ( -3.097522238704186748E-14, 59.74999999999991473, -4.499999999999967137 ) ) ;
#6027 = LINE ( 'NONE', #2485, #22703 ) ;
#6028 = DIRECTION ( 'NONE',  ( 0.000000000000000000, -6.938893903907238633E-15, -1.000000000000000000 ) ) ;
#6029 = CARTESIAN_POINT ( 'NONE',  ( 42.50000000000014921, 8.500000000000003553, -0.4999999999999726885 ) ) ;
#6030 = DIRECTION ( 'NONE',  ( -4.019602852144232182E-47, -6.982962677686261977E-15, -1.000000000000000000 ) ) ;
#6031 = ORIENTED_EDGE ( 'NONE', *, *, #6805, .F. ) ;
#6032 = EDGE_CURVE ( 'NONE', #8438, #20684, #5596, .T. ) ;
#6033 =( NAMED_UNIT ( * ) PLANE_ANGLE_UNIT ( ) SI_UNIT ( $, .RADIAN. ) );
#6035 = ORIENTED_EDGE ( 'NONE', *, *, #484, .T. ) ;
#6034 = ORIENTED_EDGE ( 'NONE', *, *, #16204, .F. ) ;
#6036 = UNCERTAINTY_MEASURE_WITH_UNIT (LENGTH_MEASURE( 1.000000000000000082E-05 ), #11281, 'distance_accuracy_value', 'NONE');
#6037 = ORIENTED_EDGE ( 'NONE', *, *, #2484, .F. ) ;
#6039 = VERTEX_POINT ( 'NONE', #7874 ) ;
#6038 = ORIENTED_EDGE ( 'NONE', *, *, #10119, .T. ) ;
#6040 = AXIS2_PLACEMENT_3D ( 'NONE', #16012, #10496, #22977 ) ;
#6041 = ORIENTED_EDGE ( 'NONE', *, *, #5936, .F. ) ;
#6042 = LINE ( 'NONE', #11437, #7260 ) ;
#6043 = ORIENTED_EDGE ( 'NONE', *, *, #10672, .F. ) ;
#6044 = VERTEX_POINT ( 'NONE', #5657 ) ;
#6045 = DIRECTION ( 'NONE',  ( -0.6819983600625073583, 0.7313537016191622442, 1.665472943098395307E-16 ) ) ;
#6046 = CARTESIAN_POINT ( 'NONE',  ( 115.1426525620553889, -6.246200939475476943, -5.999999999999928946 ) ) ;
#6047 = ADVANCED_FACE ( 'NONE', ( #6115 ), #18688, .T. ) ;
#6048 = CARTESIAN_POINT ( 'NONE',  ( 124.5000000000019469, -7.000000000000062172, 2.081668171172168513E-14 ) ) ;
#6049 = DIRECTION ( 'NONE',  ( 9.693522803355793065E-26, -5.963788443470848352E-28, -1.000000000000000000 ) ) ;
#6050 = DIRECTION ( 'NONE',  ( 0.000000000000000000, 0.000000000000000000, 1.000000000000000000 ) ) ;
#6051 = CARTESIAN_POINT ( 'NONE',  ( -89.70000000000059970, 4.857225732735059864E-14, 1.000000000000000888 ) ) ;
#6052 = CARTESIAN_POINT ( 'NONE',  ( 4.086262418390188778, -2.102635014057370189, 3.499999999999970690 ) ) ;
#6053 = CARTESIAN_POINT ( 'NONE',  ( 0.3126073911696447549, 4.041451884327383226, 0.000000000000000000 ) ) ;
#6054 = EDGE_CURVE ( 'NONE', #4755, #5817, #329, .T. ) ;
#6055 = DIRECTION ( 'NONE',  ( -1.000000000000000000, -4.440892098500626162E-16, 5.551115123125782702E-16 ) ) ;
#6056 = AXIS2_PLACEMENT_3D ( 'NONE', #6476, #11525, #15405 ) ;
#6057 = DIRECTION ( 'NONE',  ( 1.000000000000000000, 4.440892098500626162E-16, 5.551115123125782702E-16 ) ) ;
#6058 = CARTESIAN_POINT ( 'NONE',  ( -45.37157287525410254, 6.828427124746163202, 8.000000000000035527 ) ) ;
#6059 = VERTEX_POINT ( 'NONE', #20115 ) ;
#6060 = ADVANCED_FACE ( 'NONE', ( #3987 ), #18351, .T. ) ;
#6062 = ORIENTED_EDGE ( 'NONE', *, *, #12821, .T. ) ;
#6061 = VERTEX_POINT ( 'NONE', #13054 ) ;
#6063 = ORIENTED_EDGE ( 'NONE', *, *, #13859, .T. ) ;
#6064 = EDGE_CURVE ( 'NONE', #8658, #5235, #3340, .T. ) ;
#6065 = ORIENTED_EDGE ( 'NONE', *, *, #3421, .T. ) ;
#6066 = EDGE_CURVE ( 'NONE', #4871, #14655, #14218, .T. ) ;
#6067 = EDGE_CURVE ( 'NONE', #20666, #11557, #19820, .T. ) ;
#6068 = ORIENTED_EDGE ( 'NONE', *, *, #18922, .T. ) ;
#6069 = DIRECTION ( 'NONE',  ( 1.000000000000000000, 1.240809152955624894E-14, 0.000000000000000000 ) ) ;
#6070 = AXIS2_PLACEMENT_3D ( 'NONE', #11134, #103, #7608 ) ;
#6071 = CARTESIAN_POINT ( 'NONE',  ( 5.550000000291854363, 42.99999999900385461, -19.49999999999998934 ) ) ;
#6072 = ORIENTED_EDGE ( 'NONE', *, *, #15415, .T. ) ;
#6073 = CARTESIAN_POINT ( 'NONE',  ( 4.158413352280808439, -4.089743253945677282, -2.775557561562891351E-14 ) ) ;
#6074 = DIRECTION ( 'NONE',  ( -1.000000000000000000, -1.374679200952735400E-16, -3.676447422453419544E-32 ) ) ;
#6075 = CYLINDRICAL_SURFACE ( 'NONE', #8996, 2.549999999999997158 ) ;
#6076 = FACE_OUTER_BOUND ( 'NONE', #6536, .T. ) ;
#6077 = CARTESIAN_POINT ( 'NONE',  ( -7.521298409251902406, -11.75792766829873415, 8.817899680514910798 ) ) ;
#6078 = EDGE_CURVE ( 'NONE', #6815, #17750, #2689, .T. ) ;
#6079 = EDGE_CURVE ( 'NONE', #1148, #16805, #22574, .T. ) ;
#6080 = CARTESIAN_POINT ( 'NONE',  ( -4.000000000000095035, 1.941961291383484278, -0.3515519931180789981 ) ) ;
#6081 = EDGE_CURVE ( 'NONE', #14457, #21664, #3661, .T. ) ;
#6082 = LINE ( 'NONE', #22082, #13071 ) ;
#6083 = CARTESIAN_POINT ( 'NONE',  ( 0.02993401039713629655, 3.373851915354614928, 1.156317065392238774 ) ) ;
#6084 = CARTESIAN_POINT ( 'NONE',  ( 119.5756419024615269, -11.00000000000006573, 6.000000000000081712 ) ) ;
#6085 = FACE_BOUND ( 'NONE', #14559, .T. ) ;
#6087 = AXIS2_PLACEMENT_3D ( 'NONE', #10530, #14182, #3899 ) ;
#6086 = DIRECTION ( 'NONE',  ( -1.000000000000000000, 4.190823558986610327E-31, -1.733449886265890494E-32 ) ) ;
#6088 = ORIENTED_EDGE ( 'NONE', *, *, #3455, .T. ) ;
#6089 = EDGE_CURVE ( 'NONE', #20880, #746, #8924, .T. ) ;
#6090 = EDGE_CURVE ( 'NONE', #195, #10367, #1171, .T. ) ;
#6091 = VERTEX_POINT ( 'NONE', #4805 ) ;
#6092 = VERTEX_POINT ( 'NONE', #15386 ) ;
#6093 = EDGE_LOOP ( 'NONE', ( #5140, #22640, #12627, #22992 ) ) ;
#6094 = EDGE_CURVE ( 'NONE', #17638, #927, #4150, .T. ) ;
#6095 = ORIENTED_EDGE ( 'NONE', *, *, #13415, .F. ) ;
#6096 = DIRECTION ( 'NONE',  ( 1.000000000000000000, 1.910522504832140594E-31, -5.551115123125818447E-17 ) ) ;
#6097 = DIRECTION ( 'NONE',  ( -1.066786462891689527E-26, -6.656013887802287108E-31, -1.000000000000000000 ) ) ;
#6098 = EDGE_LOOP ( 'NONE', ( #14620, #17068, #5848, #6440 ) ) ;
#6099 = AXIS2_PLACEMENT_3D ( 'NONE', #1686, #14152, #7332 ) ;
#6100 = CARTESIAN_POINT ( 'NONE',  ( 6.495190528383244732, 4.999999999999935163, 3.750000000000003553 ) ) ;
#6101 = DIRECTION ( 'NONE',  ( -1.333893503340774882E-15, -2.778352770573747380E-17, -1.000000000000000000 ) ) ;
#6102 = CARTESIAN_POINT ( 'NONE',  ( -1.318389841742373392E-16, 1.618211776087849834E-15, -4.750000000000013323 ) ) ;
#6103 = ORIENTED_EDGE ( 'NONE', *, *, #18215, .T. ) ;
#6104 = B_SPLINE_CURVE_WITH_KNOTS ( 'NONE', 3,
 ( #20762, #878, #6627, #8164, #1119, #17441 ),
 .UNSPECIFIED., .F., .F.,
 ( 4, 2, 4 ),
 ( 0.002044882221487533212, 0.003063384235218495448, 0.004081886248949457251 ),
 .UNSPECIFIED. ) ;
#6105 = CARTESIAN_POINT ( 'NONE',  ( 2.775557561562891351E-14, 10.49999999999999822, -6.499999999999950262 ) ) ;
#6106 = CIRCLE ( 'NONE', #18860, 2.550000000000003819 ) ;
#6107 = LINE ( 'NONE', #19041, #22084 ) ;
#6108 = CARTESIAN_POINT ( 'NONE',  ( 3.938635139691124998, 0.7500000000000556222, -2.974447373137671047 ) ) ;
#6109 = CIRCLE ( 'NONE', #21886, 6.700000000000039257 ) ;
#6110 = CIRCLE ( 'NONE', #16225, 0.4999999999999990563 ) ;
#6111 = CARTESIAN_POINT ( 'NONE',  ( -7.733764002503129120, -0.7473006511613556890, 8.082002268151461166 ) ) ;
#6112 = CARTESIAN_POINT ( 'NONE',  ( 7.876571740167124247, -13.80606002021554701, 7.785394814391048079 ) ) ;
#6113 = DIRECTION ( 'NONE',  ( 0.3420201433256618850, 1.880337258636373401E-32, -0.9396926207859108704 ) ) ;
#6114 = CARTESIAN_POINT ( 'NONE',  ( 4.033901012036838374, 3.740908793663468845, -0.5205559028929584997 ) ) ;
#6115 = FACE_OUTER_BOUND ( 'NONE', #14514, .T. ) ;
#6116 =( NAMED_UNIT ( * ) PLANE_ANGLE_UNIT ( ) SI_UNIT ( $, .RADIAN. ) );
#6117 = VECTOR ( 'NONE', #19069, 999.9999999999998863 ) ;
#6118 = CARTESIAN_POINT ( 'NONE',  ( 3.974175853610068643, -2.726149789692980274, -2.409821656223221975 ) ) ;
#6119 = EDGE_CURVE ( 'NONE', #3000, #13876, #11865, .T. ) ;
#6120 = ITEM_DEFINED_TRANSFORMATION ( 'NONE', 'NONE', #22927,  #22115 ) ;
#6121 = CIRCLE ( 'NONE', #20775, 4.750000000000000888 ) ;
#6122 = ORIENTED_EDGE ( 'NONE', *, *, #10639, .F. ) ;
#6123 = AXIS2_PLACEMENT_3D ( 'NONE', #16038, #19466, #23001 ) ;
#6124 = CIRCLE ( 'NONE', #4598, 5.500000000000032863 ) ;
#6126 = EDGE_LOOP ( 'NONE', ( #14854, #5890, #11293, #9191 ) ) ;
#6125 = ORIENTED_EDGE ( 'NONE', *, *, #227, .T. ) ;
#6127 = CARTESIAN_POINT ( 'NONE',  ( 5.551115123125782702E-14, 3.000000000000027089, 2.500000000000071498 ) ) ;
#6128 = DIRECTION ( 'NONE',  ( 1.000000000000000000, 1.479114197289388027E-30, -2.013525853228518840E-32 ) ) ;
#6129 =( LENGTH_UNIT ( ) NAMED_UNIT ( * ) SI_UNIT ( .MILLI., .METRE. ) );
#6130 = VERTEX_POINT ( 'NONE', #13755 ) ;
#6131 = CARTESIAN_POINT ( 'NONE',  ( 4.175075985190096262, 4.120741555260251765, -2.775557561562891351E-14 ) ) ;
#6132 = CYLINDRICAL_SURFACE ( 'NONE', #9794, 0.5000000000000028866 ) ;
#6133 = CARTESIAN_POINT ( 'NONE',  ( 4.175326769692856210, -2.060699556488895468, 3.569236330973483806 ) ) ;
#6134 = CARTESIAN_POINT ( 'NONE',  ( -5.688936712956111919, 36.29949271875472050, -16.51803887880629418 ) ) ;
#6135 = CARTESIAN_POINT ( 'NONE',  ( -0.6554360035617893265, 4.240386000424037682, -5.441324518471510885 ) ) ;
#6136 = VECTOR ( 'NONE', #10791, 1000.000000000000000 ) ;
#6137 = DIRECTION ( 'NONE',  ( 1.431475090352998897E-31, -3.469446951953609061E-15, -1.000000000000000000 ) ) ;
#6138 = CIRCLE ( 'NONE', #23039, 4.499999999999988454 ) ;
#6139 = CARTESIAN_POINT ( 'NONE',  ( 42.50000000000014921, 8.000000000000003553, -0.4999999999999726885 ) ) ;
#6140 = CARTESIAN_POINT ( 'NONE',  ( -50.65685424949275983, -2.700000000000091216, -8.000000000000007105 ) ) ;
#6141 = CIRCLE ( 'NONE', #10631, 9.500000000000063949 ) ;
#6142 = CIRCLE ( 'NONE', #22297, 4.500000000000045297 ) ;
#6144 = EDGE_CURVE ( 'NONE', #14991, #13234, #12077, .T. ) ;
#6143 = AXIS2_PLACEMENT_3D ( 'NONE', #10007, #11292, #18598 ) ;
#6145 = CARTESIAN_POINT ( 'NONE',  ( -8.326672684688674053E-14, 4.999999999999893419, 7.499999999999958256 ) ) ;
#6146 = DIRECTION ( 'NONE',  ( 1.333893503340774882E-15, 2.778352770573747380E-17, 1.000000000000000000 ) ) ;
#6147 = CARTESIAN_POINT ( 'NONE',  ( 54.42435809754115894, 0.000000000000000000, 6.000000000000136779 ) ) ;
#6148 = CARTESIAN_POINT ( 'NONE',  ( -56.91911807125104872, -0.5000000000001045830, -8.333333333333413862 ) ) ;
#6149 = EDGE_CURVE ( 'NONE', #19900, #18558, #21296, .T. ) ;
#6150 = ORIENTED_EDGE ( 'NONE', *, *, #6796, .T. ) ;
#6152 = ORIENTED_EDGE ( 'NONE', *, *, #16137, .T. ) ;
#6151 = ORIENTED_EDGE ( 'NONE', *, *, #17910, .T. ) ;
#6153 = EDGE_CURVE ( 'NONE', #5825, #12740, #23208, .T. ) ;
#6154 = ORIENTED_EDGE ( 'NONE', *, *, #14240, .F. ) ;
#6155 = ORIENTED_EDGE ( 'NONE', *, *, #19160, .T. ) ;
#6156 = AXIS2_PLACEMENT_3D ( 'NONE', #2783, #10183, #2662 ) ;
#6158 = ORIENTED_EDGE ( 'NONE', *, *, #11836, .F. ) ;
#6157 = EDGE_LOOP ( 'NONE', ( #8519, #15394, #9567, #19174 ) ) ;
#6159 = CIRCLE ( 'NONE', #19295, 3.300000000000019806 ) ;
#6160 = EDGE_LOOP ( 'NONE', ( #9792, #225, #10393, #5883 ) ) ;
#6161 = VECTOR ( 'NONE', #11732, 1000.000000000000000 ) ;
#6162 = DIRECTION ( 'NONE',  ( 1.454462294001240516E-30, 1.000000000000000000, 0.000000000000000000 ) ) ;
#6163 = AXIS2_PLACEMENT_3D ( 'NONE', #16300, #12896, #14888 ) ;
#6164 = CARTESIAN_POINT ( 'NONE',  ( 22.49999999999999645, 4.250000000000031974, -0.2500000000000036637 ) ) ;
#6165 = AXIS2_PLACEMENT_3D ( 'NONE', #20712, #17160, #15282 ) ;
#6166 = ORIENTED_EDGE ( 'NONE', *, *, #19879, .T. ) ;
#6167 = CARTESIAN_POINT ( 'NONE',  ( 3.806834918298588555, 3.031088913245420180, 1.749999999999915623 ) ) ;
#6168 = CARTESIAN_POINT ( 'NONE',  ( 3.999999999999948042, 2.309401076758532678, -3.504271511726787747 ) ) ;
#6169 = DIRECTION ( 'NONE',  ( -1.000000000000000000, 1.389842848855773367E-62, -2.013525853228507892E-32 ) ) ;
#6170 = CARTESIAN_POINT ( 'NONE',  ( 2.918498775983380256E-10, 2.999999999003851503, -45.00000000000000000 ) ) ;
#6171 = CARTESIAN_POINT ( 'NONE',  ( -7.499999999999992895, -2.645898033750305522, 9.250000000000014211 ) ) ;
#6172 = EDGE_CURVE ( 'NONE', #5042, #16493, #16786, .T. ) ;
#6173 = CARTESIAN_POINT ( 'NONE',  ( 3.999999999999976019, -1.700175430507228969, -3.320327275038315484 ) ) ;
#6174 = CARTESIAN_POINT ( 'NONE',  ( 7.710998176012537897, -2.456120859166848192, 8.114728912742497968 ) ) ;
#6175 = FACE_OUTER_BOUND ( 'NONE', #22386, .T. ) ;
#6176 =( LENGTH_UNIT ( ) NAMED_UNIT ( * ) SI_UNIT ( .MILLI., .METRE. ) );
#6177 = VECTOR ( 'NONE', #3778, 1000.000000000000000 ) ;
#6178 = VECTOR ( 'NONE', #10611, 1000.000000000000114 ) ;
#6179 = CARTESIAN_POINT ( 'NONE',  ( 42.00000000000014921, 11.00000000000000000, -0.4999999999999449329 ) ) ;
#6180 = DIRECTION ( 'NONE',  ( 2.220446049250313081E-16, -1.000000000000000000, 7.025792437124636392E-31 ) ) ;
#6181 = FACE_OUTER_BOUND ( 'NONE', #21920, .T. ) ;
#6182 = AXIS2_PLACEMENT_3D ( 'NONE', #5496, #14773, #550 ) ;
#6183 = ORIENTED_EDGE ( 'NONE', *, *, #17280, .T. ) ;
#6185 = ORIENTED_EDGE ( 'NONE', *, *, #18465, .F. ) ;
#6184 = VERTEX_POINT ( 'NONE', #823 ) ;
#6186 = ORIENTED_EDGE ( 'NONE', *, *, #20019, .T. ) ;
#6187 = ORIENTED_EDGE ( 'NONE', *, *, #6794, .F. ) ;
#6188 = B_SPLINE_CURVE_WITH_KNOTS ( 'NONE', 3,
 ( #20059, #14299, #21487, #5362, #16853, #20643 ),
 .UNSPECIFIED., .F., .F.,
 ( 4, 2, 4 ),
 ( -3.640115492456156008E-06, 0.0002066546034006130211, 0.0004169493222936822025 ),
 .UNSPECIFIED. ) ;
#6189 = ORIENTED_EDGE ( 'NONE', *, *, #16707, .T. ) ;
#6190 = DIRECTION ( 'NONE',  ( 1.000000000000000000, 0.000000000000000000, 0.000000000000000000 ) ) ;
#6191 = AXIS2_PLACEMENT_3D ( 'NONE', #18347, #14689, #4207 ) ;
#6192 = CLOSED_SHELL ( 'NONE', ( #4660, #5415, #6491, #366, #21160, #20826, #7374, #23230, #14266, #2167, #11114, #22694, #9274, #19167, #3234, #7383, #13121, #20861, #9538, #15105, #6255, #2892, #20039, #5717, #4749, #2527, #13134, #15705, #14906, #18451, #15388, #12568, #8902, #10569, #5518, #5069, #7425, #22943, #6472, #11519, #15651, #7686, #19478, #16565, #18269, #8217, #20272, #11911 ) ) ;
#6193 = CARTESIAN_POINT ( 'NONE',  ( -6.000000000000088818, -2.000000000000043521, 7.500000000000076383 ) ) ;
#6194 = ORIENTED_EDGE ( 'NONE', *, *, #6670, .T. ) ;
#6195 = CARTESIAN_POINT ( 'NONE',  ( 4.071447262713891568, -4.041451884327432076, 1.040834085586084257E-14 ) ) ;
#6196 = EDGE_CURVE ( 'NONE', #18871, #13205, #15159, .T. ) ;
#6197 = CARTESIAN_POINT ( 'NONE',  ( 4.175326769692855322, 2.060699556488938544, 3.569236330973458049 ) ) ;
#6198 = CARTESIAN_POINT ( 'NONE',  ( -10.49999999999998224, -12.50000000000000711, 9.250000000000063949 ) ) ;
#6199 = CARTESIAN_POINT ( 'NONE',  ( 36.00000000029184832, 49.99999999900385461, -16.00000000000000000 ) ) ;
#6200 = CARTESIAN_POINT ( 'NONE',  ( -7.778057173929672885, -12.23790148979555070, 7.981635986975519792 ) ) ;
#6201 = CARTESIAN_POINT ( 'NONE',  ( -8.697224362268007880, -14.00000000000004619, 6.250000000000031086 ) ) ;
#6202 = DIRECTION ( 'NONE',  ( -1.000000000000000000, -4.252453317207022894E-31, 5.551115123125818447E-17 ) ) ;
#6203 = EDGE_CURVE ( 'NONE', #13307, #11319, #4564, .T. ) ;
#6204 = DIRECTION ( 'NONE',  ( 0.000000000000000000, 0.000000000000000000, 1.000000000000000000 ) ) ;
#6206 = EDGE_CURVE ( 'NONE', #6092, #6, #11743, .T. ) ;
#6205 = CARTESIAN_POINT ( 'NONE',  ( 37.69139372032820745, 3.387530319305491578E-14, -10.77870956205554975 ) ) ;
#6207 = AXIS2_PLACEMENT_3D ( 'NONE', #20111, #9633, #22224 ) ;
#6208 = CARTESIAN_POINT ( 'NONE',  ( 6.000000000291855429, -0.5000000009961480529, -3.449999999999997957 ) ) ;
#6209 = DIRECTION ( 'NONE',  ( -1.066786462891689527E-26, -6.656013887802287108E-31, -1.000000000000000000 ) ) ;
#6210 = ORIENTED_EDGE ( 'NONE', *, *, #8532, .F. ) ;
#6211 = ORIENTED_EDGE ( 'NONE', *, *, #7675, .F. ) ;
#6212 = ORIENTED_EDGE ( 'NONE', *, *, #14276, .T. ) ;
#6213 = EDGE_LOOP ( 'NONE', ( #22947, #10578, #15601 ) ) ;
#6214 = VERTEX_POINT ( 'NONE', #9995 ) ;
#6215 = CARTESIAN_POINT ( 'NONE',  ( -4.000000000000004441, 0.7862748000878184707, -5.565527722372431541 ) ) ;
#6216 = ADVANCED_FACE ( 'NONE', ( #17146 ), #17265, .T. ) ;
#6217 = FACE_OUTER_BOUND ( 'NONE', #14333, .T. ) ;
#6218 = VERTEX_POINT ( 'NONE', #4695 ) ;
#6219 = DIRECTION ( 'NONE',  ( 0.000000000000000000, 0.000000000000000000, -1.000000000000000000 ) ) ;
#6220 = CARTESIAN_POINT ( 'NONE',  ( 4.330127018922110160, -5.551115123125782702E-14, -7.499999999999996447 ) ) ;
#6221 = CARTESIAN_POINT ( 'NONE',  ( -0.5000000000000837108, 1.999999999999890754, 8.000000000000076383 ) ) ;
#6222 = EDGE_CURVE ( 'NONE', #12422, #22613, #19049, .T. ) ;
#6223 = ORIENTED_EDGE ( 'NONE', *, *, #13675, .T. ) ;
#6224 = AXIS2_PLACEMENT_3D ( 'NONE', #6014, #11522, #13416 ) ;
#6225 = CARTESIAN_POINT ( 'NONE',  ( -6.083292711304078892, 36.06725630338318211, -18.74270568520632807 ) ) ;
#6226 = DIRECTION ( 'NONE',  ( 0.000000000000000000, 1.297468594113506001E-30, 1.000000000000000000 ) ) ;
#6227 = FACE_OUTER_BOUND ( 'NONE', #14200, .T. ) ;
#6228 = CARTESIAN_POINT ( 'NONE',  ( 3.973110223767125859, 2.263145622885971846E-11, 3.565797985667392922 ) ) ;
#6229 = CARTESIAN_POINT ( 'NONE',  ( 0.000000000000000000, 0.000000000000000000, 0.000000000000000000 ) ) ;
#6230 = LINE ( 'NONE', #17028, #13058 ) ;
#6231 = EDGE_CURVE ( 'NONE', #8964, #19696, #17984, .T. ) ;
#6232 = EDGE_CURVE ( 'NONE', #21954, #11543, #22933, .T. ) ;
#6233 = DIRECTION ( 'NONE',  ( 0.000000000000000000, -1.000000000000000000, 0.000000000000000000 ) ) ;
#6234 = CARTESIAN_POINT ( 'NONE',  ( 57.49335071782242323, -0.7089083427137543580, -6.499999999999922728 ) ) ;
#6235 = CARTESIAN_POINT ( 'NONE',  ( 8.660254037844337560, 4.999999999999948486, 2.775557561562891351E-14 ) ) ;
#6236 = DIRECTION ( 'NONE',  ( -2.220446049250313081E-16, 1.000000000000000000, -7.025792437124636392E-31 ) ) ;
#6237 = ORIENTED_EDGE ( 'NONE', *, *, #5328, .T. ) ;
#6238 = EDGE_CURVE ( 'NONE', #19599, #15995, #17622, .T. ) ;
#6239 = EDGE_CURVE ( 'NONE', #4603, #4887, #20196, .T. ) ;
#6240 = EDGE_CURVE ( 'NONE', #13412, #9370, #9291, .T. ) ;
#6241 = EDGE_CURVE ( 'NONE', #8991, #8964, #15343, .T. ) ;
#6243 = VERTEX_POINT ( 'NONE', #1736 ) ;
#6242 = EDGE_LOOP ( 'NONE', ( #14049, #5136, #11701, #22584 ) ) ;
#6244 = CIRCLE ( 'NONE', #3244, 0.4999999999999995559 ) ;
#6245 = LINE ( 'NONE', #18945, #22692 ) ;
#6246 = DIRECTION ( 'NONE',  ( 4.440892098500626162E-16, 1.000000000000000000, 2.146163712481655900E-16 ) ) ;
#6247 = PLANE ( 'NONE',  #22299 ) ;
#6248 = EDGE_LOOP ( 'NONE', ( #17651, #13815, #9537, #4 ) ) ;
#6249 = CARTESIAN_POINT ( 'NONE',  ( 22.49999999999998934, 4.250000000000017764, -18.75000000000001421 ) ) ;
#6250 = EDGE_CURVE ( 'NONE', #17638, #15390, #23050, .T. ) ;
#6251 = DIRECTION ( 'NONE',  ( 1.000000000000000000, 0.000000000000000000, 0.000000000000000000 ) ) ;
#6252 = CARTESIAN_POINT ( 'NONE',  ( 37.68301270189238750, -2.676886543277417521E-15, -10.50000000000003908 ) ) ;
#6253 = CARTESIAN_POINT ( 'NONE',  ( 3.972709601346597008, -3.429395227388317924, -1.191688283765312439 ) ) ;
#6254 = DIRECTION ( 'NONE',  ( 0.000000000000000000, 1.000000000000000000, 0.000000000000000000 ) ) ;
#6255 = ADVANCED_FACE ( 'NONE', ( #12320 ), #21520, .T. ) ;
#6256 = DIRECTION ( 'NONE',  ( -3.885780586188016830E-16, -4.437342591868156373E-31, 1.000000000000000000 ) ) ;
#6257 = CARTESIAN_POINT ( 'NONE',  ( 108.2426266706970779, -6.527605602963587828, 6.000000000000109246 ) ) ;
#6258 = FILL_AREA_STYLE_COLOUR ( '', #7993 ) ;
#6260 = ADVANCED_FACE ( 'NONE', ( #10793 ), #8219, .T. ) ;
#6259 = FACE_OUTER_BOUND ( 'NONE', #1696, .T. ) ;
#6261 = DIRECTION ( 'NONE',  ( -2.013525853228507892E-32, -6.902532920683810383E-31, 1.000000000000000000 ) ) ;
#6262 = CARTESIAN_POINT ( 'NONE',  ( -7.000000000000020428, -3.018576030000264865, 8.916666666666712260 ) ) ;
#6263 = LINE ( 'NONE', #13198, #12269 ) ;
#6264 = ORIENTED_EDGE ( 'NONE', *, *, #3933, .T. ) ;
#6265 = AXIS2_PLACEMENT_3D ( 'NONE', #8657, #12176, #17594 ) ;
#6267 = ORIENTED_EDGE ( 'NONE', *, *, #9806, .F. ) ;
#6266 = ORIENTED_EDGE ( 'NONE', *, *, #186, .F. ) ;
#6268 = CIRCLE ( 'NONE', #2118, 0.5000000000000004441 ) ;
#6269 = UNCERTAINTY_MEASURE_WITH_UNIT (LENGTH_MEASURE( 1.000000000000000082E-05 ), #14842, 'distance_accuracy_value', 'NONE');
#6270 = VERTEX_POINT ( 'NONE', #19858 ) ;
#6272 = VERTEX_POINT ( 'NONE', #16078 ) ;
#6271 = ORIENTED_EDGE ( 'NONE', *, *, #22175, .F. ) ;
#6273 = LINE ( 'NONE', #984, #4988 ) ;
#6274 = DIRECTION ( 'NONE',  ( 8.659560561600564896E-17, 0.7071067811865516806, -0.7071067811865434649 ) ) ;
#6275 = ORIENTED_EDGE ( 'NONE', *, *, #1912, .F. ) ;
#6276 = DIRECTION ( 'NONE',  ( 0.000000000000000000, 0.000000000000000000, 1.000000000000000000 ) ) ;
#6277 = VECTOR ( 'NONE', #18742, 1000.000000000000000 ) ;
#6278 = CARTESIAN_POINT ( 'NONE',  ( 4.101954839143033382, 2.368264730582954947, -3.681130640444268298 ) ) ;
#6279 = PLANE ( 'NONE',  #19931 ) ;
#6280 = CARTESIAN_POINT ( 'NONE',  ( -7.778057173929718182, -1.762098510204431756, 7.981635986975294195 ) ) ;
#6281 = AXIS2_PLACEMENT_3D ( 'NONE', #20033, #5688, #12852 ) ;
#6282 = PLANE ( 'NONE',  #20844 ) ;
#6283 = AXIS2_PLACEMENT_3D ( 'NONE', #13778, #20727, #1089 ) ;
#6284 = CARTESIAN_POINT ( 'NONE',  ( 2.499999999999998668, 2.000000000000001776, -17.75000000000000711 ) ) ;
#6285 = ADVANCED_FACE ( 'NONE', ( #3512 ), #1626, .F. ) ;
#6286 = CARTESIAN_POINT ( 'NONE',  ( 7.854293383767891434, -2.312270958411924315, 7.820081954007007674 ) ) ;
#6287 = DIRECTION ( 'NONE',  ( 1.000000000000000000, 4.440892098500626162E-16, -5.551115123125782702E-16 ) ) ;
#6288 = LINE ( 'NONE', #2402, #20751 ) ;
#6289 = EDGE_CURVE ( 'NONE', #18669, #10966, #10411, .T. ) ;
#6290 = CARTESIAN_POINT ( 'NONE',  ( -4.000000000000002665, -0.3902508023145539462, -1.988833360153096802E-15 ) ) ;
#6291 = VECTOR ( 'NONE', #13402, 1000.000000000000114 ) ;
#6292 = FACE_OUTER_BOUND ( 'NONE', #5421, .T. ) ;
#6293 = CARTESIAN_POINT ( 'NONE',  ( -6.587771436282945814, 13.98878796535109359, -27.53104552455945608 ) ) ;
#6294 = CARTESIAN_POINT ( 'NONE',  ( 4.158807179406252885, 2.089320655794529635, -3.500000000000006217 ) ) ;
#6295 = ORIENTED_EDGE ( 'NONE', *, *, #217, .F. ) ;
#6296 = UNCERTAINTY_MEASURE_WITH_UNIT (LENGTH_MEASURE( 1.000000000000000082E-05 ), #21237, 'distance_accuracy_value', 'NONE');
#6297 = SURFACE_STYLE_FILL_AREA ( #9709 ) ;
#6298 = AXIS2_PLACEMENT_3D ( 'NONE', #20581, #4326, #15036 ) ;
#6300 = ORIENTED_EDGE ( 'NONE', *, *, #8934, .F. ) ;
#6299 = ORIENTED_EDGE ( 'NONE', *, *, #8397, .T. ) ;
#6301 = AXIS2_PLACEMENT_3D ( 'NONE', #2902, #6438, #13498 ) ;
#6302 = EDGE_LOOP ( 'NONE', ( #18245, #10546, #14965, #5915 ) ) ;
#6303 = VERTEX_POINT ( 'NONE', #3403 ) ;
#6304 = CIRCLE ( 'NONE', #9300, 2.500000000000002220 ) ;
#6305 = EDGE_LOOP ( 'NONE', ( #9339, #2210, #835, #14254 ) ) ;
#6306 = CARTESIAN_POINT ( 'NONE',  ( 4.114405500665259119, -2.025575754679708407, 3.508400121684940753 ) ) ;
#6307 = AXIS2_PLACEMENT_3D ( 'NONE', #1120, #17445, #6628 ) ;
#6308 = CARTESIAN_POINT ( 'NONE',  ( 81.85734743794765222, -6.246200939475254899, -5.999999999999921840 ) ) ;
#6309 = VERTEX_POINT ( 'NONE', #14450 ) ;
#6310 = VECTOR ( 'NONE', #12493, 1000.000000000000000 ) ;
#6311 = CARTESIAN_POINT ( 'NONE',  ( -50.65685424949277404, 3.200000000000022382, 8.000000000000021316 ) ) ;
#6312 = DIRECTION ( 'NONE',  ( -8.438582421954110511E-32, 0.000000000000000000, -1.000000000000000000 ) ) ;
#6313 = CARTESIAN_POINT ( 'NONE',  ( 6.938893903907228378E-15, 4.618802153517023612, -3.433295621305385126 ) ) ;
#6314 = AXIS2_PLACEMENT_3D ( 'NONE', #1846, #9034, #12557 ) ;
#6315 = CARTESIAN_POINT ( 'NONE',  ( 10.50000000000000888, -12.50000000000002842, 5.750000000000088818 ) ) ;
#6316 = CARTESIAN_POINT ( 'NONE',  ( 4.104070371397483541, 4.047367226856738220, 0.000000000000000000 ) ) ;
#6317 = CIRCLE ( 'NONE', #18331, 4.750000000000000888 ) ;
#6318 = DIRECTION ( 'NONE',  ( -1.000000000000000000, 1.337182679398780230E-14, 0.000000000000000000 ) ) ;
#6319 = CARTESIAN_POINT ( 'NONE',  ( -4.330127018922234505, 4.689110867544671102, -7.500000000000000000 ) ) ;
#6320 = CARTESIAN_POINT ( 'NONE',  ( -6.000000000000143885, 1.999999999999960032, 8.000000000000062172 ) ) ;
#6321 = DIRECTION ( 'NONE',  ( -1.000000000000000000, -1.479114197289388027E-30, 2.013525853228518840E-32 ) ) ;
#6322 = ORIENTED_EDGE ( 'NONE', *, *, #19, .F. ) ;
#6323 = PRESENTATION_STYLE_ASSIGNMENT (( #20803 ) ) ;
#6324 = DIRECTION ( 'NONE',  ( -1.066811114794976679E-26, 0.000000000000000000, -1.000000000000000000 ) ) ;
#6325 = AXIS2_PLACEMENT_3D ( 'NONE', #1316, #8484, #4939 ) ;
#6326 = DIRECTION ( 'NONE',  ( 1.000000000000000000, 1.479114197289397135E-31, 5.916456789157588541E-31 ) ) ;
#6327 = VERTEX_POINT ( 'NONE', #27 ) ;
#6328 = ADVANCED_FACE ( 'NONE', ( #5401 ), #15963, .T. ) ;
#6329 = EDGE_LOOP ( 'NONE', ( #6154, #13091, #13199, #15336 ) ) ;
#6330 = ORIENTED_EDGE ( 'NONE', *, *, #21348, .F. ) ;
#6331 = ORIENTED_EDGE ( 'NONE', *, *, #17861, .T. ) ;
#6332 = CIRCLE ( 'NONE', #17589, 4.000000000000000888 ) ;
#6333 = CARTESIAN_POINT ( 'NONE',  ( -4.000000000000052403, -2.309401076758560656, -5.000000000000000888 ) ) ;
#6334 = CARTESIAN_POINT ( 'NONE',  ( 37.00000000000014211, 0.000000000000000000, -3.000000000000002665 ) ) ;
#6335 = ORIENTED_EDGE ( 'NONE', *, *, #4067, .F. ) ;
#6336 = CARTESIAN_POINT ( 'NONE',  ( -7.500000000000020428, -6.999999999999995559, 12.24999999999999645 ) ) ;
#6337 = DIRECTION ( 'NONE',  ( -4.019602852144215652E-47, -6.982962677686261977E-15, -1.000000000000000000 ) ) ;
#6338 = DIRECTION ( 'NONE',  ( -1.000000000000000000, 1.550910762415513985E-16, 3.012982189080959477E-32 ) ) ;
#6339 = AXIS2_PLACEMENT_3D ( 'NONE', #1400, #15624, #15738 ) ;
#6340 = CARTESIAN_POINT ( 'NONE',  ( 66.26395429947831417, -6.500000000000005329, 6.000000000000192735 ) ) ;
#6341 = AXIS2_PLACEMENT_3D ( 'NONE', #22489, #6376, #15762 ) ;
#6342 = CARTESIAN_POINT ( 'NONE',  ( 4.158921614371280384, 4.076055977742235825, -0.05993604794454210349 ) ) ;
#6343 = ADVANCED_FACE ( 'NONE', ( #14096 ), #14924, .T. ) ;
#6344 = CARTESIAN_POINT ( 'NONE',  ( 124.5000000000018758, -13.52760560296373171, -6.500000000000081712 ) ) ;
#6345 = DIRECTION ( 'NONE',  ( -1.000000000000000000, 0.000000000000000000, 0.000000000000000000 ) ) ;
#6346 = CARTESIAN_POINT ( 'NONE',  ( 8.725359747074524108, -13.50000000719894366, 6.816426071237588147 ) ) ;
#6347 = DIRECTION ( 'NONE',  ( 2.168404344971017743E-16, 1.000000000000000000, -6.982962677686261977E-15 ) ) ;
#6348 = CARTESIAN_POINT ( 'NONE',  ( -1.249000902703301108E-13, -6.938893903907228378E-14, 8.000000000000062172 ) ) ;
#6349 = DIRECTION ( 'NONE',  ( 2.013525853228507892E-32, 6.902532920683810383E-31, -1.000000000000000000 ) ) ;
#6350 = EDGE_CURVE ( 'NONE', #3000, #17067, #13051, .T. ) ;
#6351 = DIRECTION ( 'NONE',  ( 9.121204216617949000E-31, 1.000000000000000000, -6.982962677686261977E-15 ) ) ;
#6352 = CIRCLE ( 'NONE', #9356, 6.500000000000005329 ) ;
#6353 = ORIENTED_EDGE ( 'NONE', *, *, #2212, .F. ) ;
#6354 = EDGE_CURVE ( 'NONE', #902, #18520, #19384, .T. ) ;
#6355 = VECTOR ( 'NONE', #13252, 1000.000000000000114 ) ;
#6356 = CONTEXT_DEPENDENT_SHAPE_REPRESENTATION ( #5346, #8556 ) ;
#6357 = AXIS2_PLACEMENT_3D ( 'NONE', #14893, #560, #7839 ) ;
#6358 = ORIENTED_EDGE ( 'NONE', *, *, #17948, .F. ) ;
#6361 = VERTEX_POINT ( 'NONE', #22402 ) ;
#6360 = EDGE_CURVE ( 'NONE', #15244, #5077, #3285, .T. ) ;
#6359 = ORIENTED_EDGE ( 'NONE', *, *, #8983, .T. ) ;
#6362 = EDGE_CURVE ( 'NONE', #10913, #7460, #11021, .T. ) ;
#6363 = DIRECTION ( 'NONE',  ( -0.8571428571428572063, 6.547888496751957777E-15, 0.5150787536377126052 ) ) ;
#6364 = ADVANCED_FACE ( 'NONE', ( #8049 ), #16859, .T. ) ;
#6365 = CARTESIAN_POINT ( 'NONE',  ( 1.999999999999944045, -3.464101615137820112, -3.142992957459231462 ) ) ;
#6366 =( NAMED_UNIT ( * ) SI_UNIT ( $, .STERADIAN. ) SOLID_ANGLE_UNIT ( ) );
#6367 = ORIENTED_EDGE ( 'NONE', *, *, #11092, .T. ) ;
#6368 = CARTESIAN_POINT ( 'NONE',  ( -3.200000000000091660, -2.000000000000050182, -7.500000000000034639 ) ) ;
#6369 = CARTESIAN_POINT ( 'NONE',  ( 42.00000000000014921, 8.000000000000003553, -15.00000000000001421 ) ) ;
#6370 = CARTESIAN_POINT ( 'NONE',  ( 0.000000000000000000, 1.749999999999973799, 4.749999999999997335 ) ) ;
#6371 = DIRECTION ( 'NONE',  ( -1.000000000000000000, 7.477632011778292156E-48, -3.885780586188017323E-16 ) ) ;
#6372 = CIRCLE ( 'NONE', #14624, 7.500000000000001776 ) ;
#6373 = CARTESIAN_POINT ( 'NONE',  ( 0.000000000000000000, 3.031088913245508110, -1.750000000000029310 ) ) ;
#6374 = PLANE ( 'NONE',  #19987 ) ;
#6375 = PLANE ( 'NONE',  #5442 ) ;
#6376 = DIRECTION ( 'NONE',  ( -7.860214984770699307E-18, 1.409037165336591006E-16, 1.000000000000000000 ) ) ;
#6377 = CARTESIAN_POINT ( 'NONE',  ( -4.483790972161962429, 0.7500000000000504041, -2.619109171265773917 ) ) ;
#6378 = ADVANCED_FACE ( 'NONE', ( #21851 ), #3841, .T. ) ;
#6379 = EDGE_CURVE ( 'NONE', #7024, #9098, #9813, .T. ) ;
#6380 = DIRECTION ( 'NONE',  ( -1.387778780781450803E-15, 0.000000000000000000, 1.000000000000000000 ) ) ;
#6381 = AXIS2_PLACEMENT_3D ( 'NONE', #14234, #5529, #19984 ) ;
#6382 = CARTESIAN_POINT ( 'NONE',  ( 0.000000000000000000, 0.000000000000000000, 0.000000000000000000 ) ) ;
#6383 = CARTESIAN_POINT ( 'NONE',  ( 1.387778780781445676E-14, 4.857225732735059864E-14, -1.500000000000001332 ) ) ;
#6384 = AXIS2_PLACEMENT_3D ( 'NONE', #6840, #1773, #21207 ) ;
#6385 = ORIENTED_EDGE ( 'NONE', *, *, #10223, .F. ) ;
#6386 =( NAMED_UNIT ( * ) SI_UNIT ( $, .STERADIAN. ) SOLID_ANGLE_UNIT ( ) );
#6388 = VERTEX_POINT ( 'NONE', #9936 ) ;
#6387 = EDGE_LOOP ( 'NONE', ( #14332, #10250, #18668, #10996 ) ) ;
#6389 = ADVANCED_FACE ( 'NONE', ( #22285 ), #4780, .T. ) ;
#6390 = VERTEX_POINT ( 'NONE', #6179 ) ;
#6393 = EDGE_LOOP ( 'NONE', ( #2115, #4280, #2726, #13208 ) ) ;
#6392 = ADVANCED_FACE ( 'NONE', ( #22519 ), #11453, .F. ) ;
#6391 = ORIENTED_EDGE ( 'NONE', *, *, #22914, .F. ) ;
#6394 = DIRECTION ( 'NONE',  ( 0.000000000000000000, 0.000000000000000000, -1.000000000000000000 ) ) ;
#6395 = ADVANCED_FACE ( 'NONE', ( #6292 ), #21385, .T. ) ;
#6396 = DIRECTION ( 'NONE',  ( -0.6819983600624981435, -0.7313537016191709039, 0.000000000000000000 ) ) ;
#6397 = PRESENTATION_STYLE_ASSIGNMENT (( #2624 ) ) ;
#6398 = CARTESIAN_POINT ( 'NONE',  ( -55.25320565519148630, -2.775557561562891351E-14, 7.500000000000007105 ) ) ;
#6399 = DIRECTION ( 'NONE',  ( 2.220446049250313081E-16, -1.000000000000000000, 7.025792437124636392E-31 ) ) ;
#6400 = FACE_OUTER_BOUND ( 'NONE', #23021, .T. ) ;
#6401 = CARTESIAN_POINT ( 'NONE',  ( -6.000000000000116351, 7.999999999999958256, -7.500000000000062172 ) ) ;
#6402 = CARTESIAN_POINT ( 'NONE',  ( 0.2500000000000036637, 2.000000000000001776, -17.00000000000000711 ) ) ;
#6403 = CARTESIAN_POINT ( 'NONE',  ( 3.999999999999975131, -2.471525695159832559, -3.686886880705775305 ) ) ;
#6404 = CARTESIAN_POINT ( 'NONE',  ( 7.120027569165277903, -2.450222941140161037, 8.099087005775102099 ) ) ;
#6405 = CARTESIAN_POINT ( 'NONE',  ( -6.000000000000074607, 7.999999999999958256, 7.500000000000062172 ) ) ;
#6406 = PLANE ( 'NONE',  #5345 ) ;
#6407 = LINE ( 'NONE', #22284, #19079 ) ;
#6408 = DIRECTION ( 'NONE',  ( 1.000000000000000000, 2.699383410053119644E-30, 3.330669073875432643E-16 ) ) ;
#6409 = CARTESIAN_POINT ( 'NONE',  ( -6.999999999708145459, 13.99999999900385106, -26.20210501113198376 ) ) ;
#6410 = CARTESIAN_POINT ( 'NONE',  ( 66.26395429947838522, 0.000000000000000000, 6.500000000000144773 ) ) ;
#6411 = ORIENTED_EDGE ( 'NONE', *, *, #20428, .T. ) ;
#6412 = AXIS2_PLACEMENT_3D ( 'NONE', #6619, #10263, #15779 ) ;
#6414 = EDGE_LOOP ( 'NONE', ( #6778, #5199, #19809, #861 ) ) ;
#6413 = VERTEX_POINT ( 'NONE', #4387 ) ;
#6415 = ADVANCED_FACE ( 'NONE', ( #20764 ), #13804, .T. ) ;
#6416 = ORIENTED_EDGE ( 'NONE', *, *, #18922, .F. ) ;
#6417 = ORIENTED_EDGE ( 'NONE', *, *, #6455, .T. ) ;
#6418 = B_SPLINE_CURVE_WITH_KNOTS ( 'NONE', 3,
 ( #10295, #16158, #14298, #12169, #1475 ),
 .UNSPECIFIED., .F., .F.,
 ( 4, 1, 4 ),
 ( 0.000000000000000000, 0.002020725942163693108, 0.004041451884327386217 ),
 .UNSPECIFIED. ) ;
#6419 = ORIENTED_EDGE ( 'NONE', *, *, #18305, .F. ) ;
#6420 = ADVANCED_FACE ( 'NONE', ( #2638 ), #20647, .T. ) ;
#6421 = VERTEX_POINT ( 'NONE', #5629 ) ;
#6422 = CARTESIAN_POINT ( 'NONE',  ( 4.170895651974856122, -2.054890354522733720, 3.559174498016319799 ) ) ;
#6423 = DIRECTION ( 'NONE',  ( 6.621482934330019970E-16, 0.8660254037844381525, -0.5000000000000008882 ) ) ;
#6424 = ORIENTED_EDGE ( 'NONE', *, *, #2608, .T. ) ;
#6425 = CARTESIAN_POINT ( 'NONE',  ( -3.999999999708153453, 35.99999999900384751, -15.50000000000000000 ) ) ;
#6426 = DIRECTION ( 'NONE',  ( -2.775557561562883955E-17, 3.406761633869148826E-16, -1.000000000000000000 ) ) ;
#6427 = DIRECTION ( 'NONE',  ( -1.000000000000000000, 0.000000000000000000, 0.000000000000000000 ) ) ;
#6428 = FACE_OUTER_BOUND ( 'NONE', #4251, .T. ) ;
#6429 = VECTOR ( 'NONE', #2952, 1000.000000000000000 ) ;
#6430 = DIRECTION ( 'NONE',  ( -9.693457064947022734E-26, 0.000000000000000000, 1.000000000000000000 ) ) ;
#6431 = CARTESIAN_POINT ( 'NONE',  ( -7.467942433933816737, -11.84606835491527121, 7.356484134531112495 ) ) ;
#6432 = CARTESIAN_POINT ( 'NONE',  ( -7.573440241539870499, -13.88616620752087982, 7.421600184846463222 ) ) ;
#6433 = PLANE ( 'NONE',  #2216 ) ;
#6434 = FACE_OUTER_BOUND ( 'NONE', #6093, .T. ) ;
#6435 = DIRECTION ( 'NONE',  ( 0.000000000000000000, 0.000000000000000000, 1.000000000000000000 ) ) ;
#6436 = ORIENTED_EDGE ( 'NONE', *, *, #9672, .F. ) ;
#6437 = CARTESIAN_POINT ( 'NONE',  ( 3.972066048304799146, 3.435565134476613824, 1.180968096049749061 ) ) ;
#6438 = DIRECTION ( 'NONE',  ( -2.013525853228507892E-32, -6.902532920683810383E-31, 1.000000000000000000 ) ) ;
#6439 = ORIENTED_EDGE ( 'NONE', *, *, #21749, .T. ) ;
#6440 = ORIENTED_EDGE ( 'NONE', *, *, #4516, .T. ) ;
#6441 = AXIS2_PLACEMENT_3D ( 'NONE', #18454, #22455, #7868 ) ;
#6442 = PRESENTATION_LAYER_ASSIGNMENT (  '', '', ( #13579 ) ) ;
#6443 = VERTEX_POINT ( 'NONE', #999 ) ;
#6444 = EDGE_CURVE ( 'NONE', #9536, #16601, #19485, .T. ) ;
#6445 = VERTEX_POINT ( 'NONE', #12788 ) ;
#6446 = PLANE ( 'NONE',  #23025 ) ;
#6447 = DIRECTION ( 'NONE',  ( -0.7313537016191746787, 0.6819983600624942577, -1.502534341919913292E-15 ) ) ;
#6448 = EDGE_LOOP ( 'NONE', ( #20248, #15947, #20566, #15318, #7290, #11405 ) ) ;
#6449 = CARTESIAN_POINT ( 'NONE',  ( 0.000000000000000000, 0.000000000000000000, -5.600000000000000533 ) ) ;
#6450 = CARTESIAN_POINT ( 'NONE',  ( 30.15500000000000114, 2.775557561562891351E-14, -2.081668171172168513E-14 ) ) ;
#6451 = CARTESIAN_POINT ( 'NONE',  ( 12.84999999999997300, -12.00000000000002842, 6.250000000000019540 ) ) ;
#6452 = DIRECTION ( 'NONE',  ( -1.000000000000000000, -2.699383410053119644E-30, -3.330669073875432643E-16 ) ) ;
#6453 = CARTESIAN_POINT ( 'NONE',  ( 4.630153689607049650, 0.000000000000000000, -3.469446951953614189E-15 ) ) ;
#6454 = CARTESIAN_POINT ( 'NONE',  ( -42.54314575050799618, 3.999999999999996447, 8.000000000000035527 ) ) ;
#6455 = EDGE_CURVE ( 'NONE', #20477, #22552, #879, .T. ) ;
#6456 = LINE ( 'NONE', #9872, #14092 ) ;
#6457 = DIRECTION ( 'NONE',  ( 1.000000000000000000, 3.469446951953617344E-15, 0.000000000000000000 ) ) ;
#6458 = CIRCLE ( 'NONE', #15825, 0.4999999999999995559 ) ;
#6459 = AXIS2_PLACEMENT_3D ( 'NONE', #574, #2324, #9502 ) ;
#6460 = LINE ( 'NONE', #20934, #15526 ) ;
#6461 = CARTESIAN_POINT ( 'NONE',  ( 0.6543461111163482169, 4.241015250120811153, -0.1391502195351433935 ) ) ;
#6462 = LINE ( 'NONE', #6235, #20897 ) ;
#6463 = B_SPLINE_CURVE_WITH_KNOTS ( 'NONE', 3,
 ( #7520, #21869, #5762, #12927, #20105, #10577 ),
 .UNSPECIFIED., .F., .F.,
 ( 4, 2, 4 ),
 ( -3.640115492385053097E-06, 0.0002066546034006847140, 0.0004169493222937545188 ),
 .UNSPECIFIED. ) ;
#6464 = CARTESIAN_POINT ( 'NONE',  ( 33.94974746859769255, 21.94974746730969528, -15.99999999999999289 ) ) ;
#6465 = ORIENTED_EDGE ( 'NONE', *, *, #5513, .F. ) ;
#6467 = VERTEX_POINT ( 'NONE', #19969 ) ;
#6466 = VERTEX_POINT ( 'NONE', #2081 ) ;
#6468 = CIRCLE ( 'NONE', #18488, 2.999999999999999112 ) ;
#6469 = FACE_OUTER_BOUND ( 'NONE', #20742, .T. ) ;
#6470 = AXIS2_PLACEMENT_3D ( 'NONE', #14542, #8068, #11704 ) ;
#6471 = LINE ( 'NONE', #8241, #12593 ) ;
#6472 = ADVANCED_FACE ( 'NONE', ( #9155 ), #16407, .T. ) ;
#6473 = DIRECTION ( 'NONE',  ( -4.440892098500626162E-16, -1.000000000000000000, -2.146163712481655900E-16 ) ) ;
#6474 = EDGE_LOOP ( 'NONE', ( #12718, #13781, #12949, #14861 ) ) ;
#6475 = DIRECTION ( 'NONE',  ( 0.000000000000000000, 0.000000000000000000, 1.000000000000000000 ) ) ;
#6476 = CARTESIAN_POINT ( 'NONE',  ( 30.00000000029184832, -9.961476088449217059E-10, -39.00000000000000000 ) ) ;
#6477 = PRODUCT ( 'slotted pan head screw_bsi_BS EN ISO 1580 - M5 x 25 - 25N', 'slotted pan head screw_bsi_BS EN ISO 1580 - M5 x 25 - 25N', '', ( #16459 ) ) ;
#6478 = ADVANCED_FACE ( 'NONE', ( #7503 ), #5550, .T. ) ;
#6479 = DIRECTION ( 'NONE',  ( -5.551115123561405253E-17, -1.000000000000000000, -2.256980353643891447E-27 ) ) ;
#6480 = AXIS2_PLACEMENT_3D ( 'NONE', #8403, #21230, #13575 ) ;
#6481 = FACE_OUTER_BOUND ( 'NONE', #4992, .T. ) ;
#6482 = DIRECTION ( 'NONE',  ( 3.885780586188016830E-16, 4.437342591868156373E-31, -1.000000000000000000 ) ) ;
#6483 = CARTESIAN_POINT ( 'NONE',  ( -5.755030100168395711E-15, -9.999999999999964473, -12.50000000000003375 ) ) ;
#6484 = CARTESIAN_POINT ( 'NONE',  ( -4.560231799112663964, 0.7500000000000501821, -2.508055037556191635 ) ) ;
#6485 = EDGE_CURVE ( 'NONE', #8753, #4567, #2161, .T. ) ;
#6486 = B_SPLINE_CURVE_WITH_KNOTS ( 'NONE', 3,
 ( #11627, #22814, #8229, #11744, #15268 ),
 .UNSPECIFIED., .F., .F.,
 ( 4, 1, 4 ),
 ( 0.000000000000000000, 0.002309401076758508826, 0.004618802153517017652 ),
 .UNSPECIFIED. ) ;
#6487 = CARTESIAN_POINT ( 'NONE',  ( 80.70499590015747060, -5.171615745951873677, 6.000000000000150990 ) ) ;
#6488 = AXIS2_PLACEMENT_3D ( 'NONE', #16156, #7241, #9231 ) ;
#6489 = DIRECTION ( 'NONE',  ( -1.066788928082016908E-26, 6.656013887802287108E-31, 1.000000000000000000 ) ) ;
#6490 = AXIS2_PLACEMENT_3D ( 'NONE', #231, #12802, #2091 ) ;
#6491 = ADVANCED_FACE ( 'NONE', ( #19211 ), #12145, .F. ) ;
#6492 = VERTEX_POINT ( 'NONE', #3229 ) ;
#6493 = VECTOR ( 'NONE', #22442, 1000.000000000000114 ) ;
#6494 = DIRECTION ( 'NONE',  ( 0.6838270277705142952, -0.7296441571687837246, -4.036486212576130633E-16 ) ) ;
#6496 = VERTEX_POINT ( 'NONE', #12024 ) ;
#6495 = EDGE_LOOP ( 'NONE', ( #7832, #19526, #1543, #12714, #17961, #8028 ) ) ;
#6497 = VERTEX_POINT ( 'NONE', #6747 ) ;
#6499 = VERTEX_POINT ( 'NONE', #6521 ) ;
#6498 = EDGE_LOOP ( 'NONE', ( #19056, #15341, #22145, #7003 ) ) ;
#6500 = ORIENTED_EDGE ( 'NONE', *, *, #18462, .T. ) ;
#6501 = CARTESIAN_POINT ( 'NONE',  ( 3.973514160553446306, 2.741076955031306550, 2.383932505289861670 ) ) ;
#6502 = CARTESIAN_POINT ( 'NONE',  ( -4.550510256924974684, 36.49999999900384751, -19.50000000000000355 ) ) ;
#6503 = EDGE_CURVE ( 'NONE', #8523, #14991, #18685, .T. ) ;
#6504 = CARTESIAN_POINT ( 'NONE',  ( 3.951447005078449148, 3.704664227300095813, 0.5833333333333124981 ) ) ;
#6505 = EDGE_CURVE ( 'NONE', #20279, #22431, #23229, .T. ) ;
#6506 = CIRCLE ( 'NONE', #14455, 0.5000000000000017764 ) ;
#6507 = VECTOR ( 'NONE', #3069, 1000.000000000000000 ) ;
#6508 = DIRECTION ( 'NONE',  ( 9.121204216617949000E-31, 1.000000000000000000, -6.982962677686261977E-15 ) ) ;
#6509 = FACE_OUTER_BOUND ( 'NONE', #205, .T. ) ;
#6510 = AXIS2_PLACEMENT_3D ( 'NONE', #8467, #6943, #21289 ) ;
#6511 = DIRECTION ( 'NONE',  ( 1.000000000000000000, 0.000000000000000000, 0.000000000000000000 ) ) ;
#6513 = ADVANCED_FACE ( 'NONE', ( #10506 ), #3106, .T. ) ;
#6512 = VECTOR ( 'NONE', #3213, 1000.000000000000000 ) ;
#6514 = CARTESIAN_POINT ( 'NONE',  ( 3.973110223768740568, -0.6864646529411670972, -3.565797985667483072 ) ) ;
#6515 = FACE_OUTER_BOUND ( 'NONE', #20381, .T. ) ;
#6516 = CARTESIAN_POINT ( 'NONE',  ( 7.734741761309861907, -2.069990213851688132, 7.004299047562906111 ) ) ;
#6517 = CARTESIAN_POINT ( 'NONE',  ( -65.47859922179033276, 0.5000000000000490719, -11.38422848940298593 ) ) ;
#6518 = DIRECTION ( 'NONE',  ( 1.000000000000000000, 1.479114197289397135E-31, 5.916456789157588541E-31 ) ) ;
#6519 = DIRECTION ( 'NONE',  ( 1.066786462891689527E-26, 6.656013887802287108E-31, 1.000000000000000000 ) ) ;
#6520 = EDGE_CURVE ( 'NONE', #17658, #21696, #2990, .T. ) ;
#6521 = CARTESIAN_POINT ( 'NONE',  ( -4.000000000000003553, 0.000000000000000000, 0.000000000000000000 ) ) ;
#6522 = DIRECTION ( 'NONE',  ( 0.000000000000000000, -1.000000000000000000, 0.000000000000000000 ) ) ;
#6523 = CARTESIAN_POINT ( 'NONE',  ( -1.387778780781445676E-14, 2.775557561562891351E-14, 12.24999999999996980 ) ) ;
#6524 = ORIENTED_EDGE ( 'NONE', *, *, #2322, .F. ) ;
#6525 = CIRCLE ( 'NONE', #19671, 6.000000000000063061 ) ;
#6526 = SURFACE_STYLE_FILL_AREA ( #4632 ) ;
#6527 = VECTOR ( 'NONE', #17522, 1000.000000000000000 ) ;
#6529 = ORIENTED_EDGE ( 'NONE', *, *, #19743, .F. ) ;
#6528 = ORIENTED_EDGE ( 'NONE', *, *, #13280, .F. ) ;
#6530 = TOROIDAL_SURFACE ( 'NONE', #10262, 9.499999999999998224, 0.5000000000000000000 ) ;
#6531 = AXIS2_PLACEMENT_3D ( 'NONE', #3272, #12187, #18202 ) ;
#6532 = VECTOR ( 'NONE', #14801, 1000.000000000000114 ) ;
#6533 = ORIENTED_EDGE ( 'NONE', *, *, #17152, .T. ) ;
#6534 = CIRCLE ( 'NONE', #3144, 0.4999999999999987232 ) ;
#6535 = EDGE_CURVE ( 'NONE', #6091, #8927, #14554, .T. ) ;
#6536 = EDGE_LOOP ( 'NONE', ( #22686, #4258, #17009, #5635 ) ) ;
#6537 = ORIENTED_EDGE ( 'NONE', *, *, #13870, .T. ) ;
#6538 = EDGE_CURVE ( 'NONE', #2294, #13206, #17319, .T. ) ;
#6539 = VERTEX_POINT ( 'NONE', #1565 ) ;
#6540 = DIRECTION ( 'NONE',  ( -1.550910762415566494E-16, -1.000000000000000000, 8.135128085091684243E-31 ) ) ;
#6541 = EDGE_CURVE ( 'NONE', #22613, #13556, #15107, .T. ) ;
#6542 = DIRECTION ( 'NONE',  ( -0.6819983600624989206, -0.7313537016191700157, 0.000000000000000000 ) ) ;
#6543 = ORIENTED_EDGE ( 'NONE', *, *, #8373, .F. ) ;
#6544 = CARTESIAN_POINT ( 'NONE',  ( 0.000000000000000000, 0.000000000000000000, 3.469446951953614189E-15 ) ) ;
#6545 = DIRECTION ( 'NONE',  ( 2.172745813409349776E-17, -1.000000000000000000, 1.309377075419428048E-16 ) ) ;
#6546 = CIRCLE ( 'NONE', #20833, 0.5000000000000029976 ) ;
#6547 = FACE_OUTER_BOUND ( 'NONE', #12234, .T. ) ;
#6548 = CIRCLE ( 'NONE', #8793, 0.5000000000000028866 ) ;
#6549 = DIRECTION ( 'NONE',  ( 6.938893903907255199E-15, 1.000000000000000000, 1.158639454543361089E-30 ) ) ;
#6550 = EDGE_CURVE ( 'NONE', #18197, #22258, #8405, .T. ) ;
#6551 = CIRCLE ( 'NONE', #15931, 4.582731094065982447 ) ;
#6552 = CARTESIAN_POINT ( 'NONE',  ( 42.50000000000020606, 2.999999999999999112, 5.551115123125782702E-14 ) ) ;
#6553 = CARTESIAN_POINT ( 'NONE',  ( -6.892555770682806857E-14, 4.999999999999976907, 4.749999999999958256 ) ) ;
#6554 = FACE_OUTER_BOUND ( 'NONE', #17457, .T. ) ;
#6555 = CARTESIAN_POINT ( 'NONE',  ( 2.918498775983380256E-10, 5.999999999003851059, -15.99999999999999289 ) ) ;
#6556 =( REPRESENTATION_RELATIONSHIP ('NONE','NONE', #19450, #17992 ) REPRESENTATION_RELATIONSHIP_WITH_TRANSFORMATION ( #12444 )SHAPE_REPRESENTATION_RELATIONSHIP( ) );
#6557 = DIRECTION ( 'NONE',  ( 0.000000000000000000, -1.000000000000000000, 0.000000000000000000 ) ) ;
#6558 = EDGE_CURVE ( 'NONE', #21116, #21352, #15306, .T. ) ;
#6559 = EDGE_LOOP ( 'NONE', ( #18846, #16196, #5441, #17131 ) ) ;
#6560 = DIRECTION ( 'NONE',  ( -0.5150787536377134934, 0.000000000000000000, -0.8571428571428567622 ) ) ;
#6561 = CARTESIAN_POINT ( 'NONE',  ( 54.42435809754118736, 2.499999999999946709, -6.499999999999922728 ) ) ;
#6562 = ORIENTED_EDGE ( 'NONE', *, *, #9580, .F. ) ;
#6563 = AXIS2_PLACEMENT_3D ( 'NONE', #19682, #3444, #14148 ) ;
#6564 = EDGE_LOOP ( 'NONE', ( #20540, #1234, #5843, #20194, #6424, #9621 ) ) ;
#6565 = CLOSED_SHELL ( 'NONE', ( #15538, #16429, #21425, #18151, #12028, #9072, #8965, #19303, #7525, #10249, #12846, #1605, #222, #22483, #11251, #5636, #14567, #12067, #14106, #18438, #5445, #18139, #3413, #12359, #11997, #337, #13861, #21460, #19463, #14837, #1069, #5526, #473, #19281, #5670, #1591, #10545, #10280, #3518, #20895, #5820, #11442, #18588, #11133, #23110, #10309, #21766, #4331, #3623, #8681, #6328, #16172, #15187, #9255, #20326, #5070, #3182 ) ) ;
#6566 = VECTOR ( 'NONE', #12938, 1000.000000000000114 ) ;
#6567 = ORIENTED_EDGE ( 'NONE', *, *, #11402, .T. ) ;
#6568 = AXIS2_PLACEMENT_3D ( 'NONE', #8039, #15201, #4261 ) ;
#6569 = ORIENTED_EDGE ( 'NONE', *, *, #5328, .F. ) ;
#6570 = PLANE ( 'NONE',  #17758 ) ;
#6571 = CARTESIAN_POINT ( 'NONE',  ( 82.19834661797897013, -5.880524088665628923, -5.999999999999943157 ) ) ;
#6572 = ORIENTED_EDGE ( 'NONE', *, *, #21155, .T. ) ;
#6573 = DIRECTION ( 'NONE',  ( 3.254448077146059901E-32, 1.000000000000000000, 6.409494854920712161E-31 ) ) ;
#6574 = CARTESIAN_POINT ( 'NONE',  ( 3.000000000291852764, 42.99999999900385461, -19.00000000000000355 ) ) ;
#6575 = CARTESIAN_POINT ( 'NONE',  ( 0.000000000000000000, 0.6000000000000137446, 4.749999999999990230 ) ) ;
#6576 = LINE ( 'NONE', #15378, #5023 ) ;
#6577 = CARTESIAN_POINT ( 'NONE',  ( 36.00000000029184832, 2.999999999003851503, -32.00000000000000000 ) ) ;
#6578 = CARTESIAN_POINT ( 'NONE',  ( -7.568268608011889498, -0.4673147976723305286, 8.579161250779817394 ) ) ;
#6579 = ADVANCED_FACE ( 'NONE', ( #15565 ), #8287, .T. ) ;
#6580 = DIRECTION ( 'NONE',  ( 2.242473278838646163E-61, 7.395570986447005381E-32, 1.000000000000000000 ) ) ;
#6581 = AXIS2_PLACEMENT_3D ( 'NONE', #9895, #21071, #22837 ) ;
#6582 = DIRECTION ( 'NONE',  ( -4.190823558986625216E-31, 1.000000000000000000, -4.190823558986625216E-31 ) ) ;
#6583 = AXIS2_PLACEMENT_3D ( 'NONE', #751, #7916, #15074 ) ;
#6584 = CARTESIAN_POINT ( 'NONE',  ( -56.87767137932630845, 1.040834085586084257E-13, 8.833333333333415638 ) ) ;
#6585 = DIRECTION ( 'NONE',  ( -2.172745813409349776E-17, 1.000000000000000000, -1.309377075419428048E-16 ) ) ;
#6586 = EDGE_CURVE ( 'NONE', #2826, #4062, #12848, .T. ) ;
#6587 = DIRECTION ( 'NONE',  ( 1.454462294001240516E-30, 1.000000000000000000, 0.000000000000000000 ) ) ;
#6588 = ORIENTED_EDGE ( 'NONE', *, *, #22056, .T. ) ;
#6590 = ORIENTED_EDGE ( 'NONE', *, *, #17260, .T. ) ;
#6589 = EDGE_LOOP ( 'NONE', ( #6035, #10167, #20949, #22027 ) ) ;
#6591 = VERTEX_POINT ( 'NONE', #2024 ) ;
#6592 = CYLINDRICAL_SURFACE ( 'NONE', #15894, 2.550000000000010481 ) ;
#6593 = FILL_AREA_STYLE_COLOUR ( '', #970 ) ;
#6594 = LINE ( 'NONE', #13768, #10867 ) ;
#6595 = ORIENTED_EDGE ( 'NONE', *, *, #1471, .T. ) ;
#6596 = DIRECTION ( 'NONE',  ( 1.000000000000000000, 2.220446049250313081E-16, -3.656342123407104498E-48 ) ) ;
#6597 = LINE ( 'NONE', #19290, #21395 ) ;
#6598 = DIRECTION ( 'NONE',  ( 0.6819983600625072473, 0.7313537016191623552, 0.000000000000000000 ) ) ;
#6599 = LINE ( 'NONE', #13774, #17385 ) ;
#6600 = CYLINDRICAL_SURFACE ( 'NONE', #3928, 4.000000000000023981 ) ;
#6601 = B_SPLINE_CURVE_WITH_KNOTS ( 'NONE', 3,
 ( #1449, #8623, #163, #18038, #8980, #19797, #1900, #5329 ),
 .UNSPECIFIED., .F., .F.,
 ( 4, 2, 2, 4 ),
 ( 0.002775112046896986880, 0.003466237704215396551, 0.004157363361533805354, 0.005539614676170624696 ),
 .UNSPECIFIED. ) ;
#6602 = DIRECTION ( 'NONE',  ( 3.885780586188016830E-16, 4.437342591868156373E-31, -1.000000000000000000 ) ) ;
#6603 = CARTESIAN_POINT ( 'NONE',  ( -89.70000000000057128, -6.245004513516505540E-14, -2.000000000000001776 ) ) ;
#6604 = CARTESIAN_POINT ( 'NONE',  ( -3.938125153161836423, 0.7500000000000509592, -2.974627600405583383 ) ) ;
#6605 = CARTESIAN_POINT ( 'NONE',  ( -7.000000000000006217, -5.999999999999987566, 10.24999999999998224 ) ) ;
#6606 = ORIENTED_EDGE ( 'NONE', *, *, #17536, .T. ) ;
#6607 = CARTESIAN_POINT ( 'NONE',  ( -41.35224048322569246, 56.99182317673109566, 43.66570243528391160 ) ) ;
#6609 = ORIENTED_EDGE ( 'NONE', *, *, #3375, .F. ) ;
#6608 = ORIENTED_EDGE ( 'NONE', *, *, #6796, .F. ) ;
#6610 = AXIS2_PLACEMENT_3D ( 'NONE', #21774, #20116, #22230 ) ;
#6611 = EDGE_CURVE ( 'NONE', #18843, #5583, #5935, .T. ) ;
#6612 = ORIENTED_EDGE ( 'NONE', *, *, #11577, .T. ) ;
#6614 = VERTEX_POINT ( 'NONE', #16482 ) ;
#6613 = ORIENTED_EDGE ( 'NONE', *, *, #2062, .F. ) ;
#6615 = CARTESIAN_POINT ( 'NONE',  ( -4.000000000000003553, 0.3904826640788006675, -2.023985227464150660E-15 ) ) ;
#6616 = DIRECTION ( 'NONE',  ( -1.095614826932724588E-15, -6.741645191078037727E-32, 1.000000000000000000 ) ) ;
#6617 = DIRECTION ( 'NONE',  ( -1.000000000000000000, -0.000000000000000000, -0.000000000000000000 ) ) ;
#6618 = CARTESIAN_POINT ( 'NONE',  ( -10.49999999999998224, -12.50000000000000711, 9.250000000000063949 ) ) ;
#6619 = CARTESIAN_POINT ( 'NONE',  ( -64.00000000000045475, 3.200000000000057021, -1.999999999999974021 ) ) ;
#6620 = CARTESIAN_POINT ( 'NONE',  ( 25.00000000000001776, 1.250000000000028866, -2.081668171172168513E-14 ) ) ;
#6621 = LINE ( 'NONE', #15557, #22713 ) ;
#6622 = CARTESIAN_POINT ( 'NONE',  ( 37.00000000000014211, 0.000000000000000000, -3.000000000000002665 ) ) ;
#6623 = CARTESIAN_POINT ( 'NONE',  ( -2.000000000000119904, -3.464101615137792134, -1.040834085586084257E-14 ) ) ;
#6624 = EDGE_CURVE ( 'NONE', #7917, #19419, #13823, .T. ) ;
#6625 = CARTESIAN_POINT ( 'NONE',  ( 12.49999999999992362, 1.250000000000015099, -9.500000000000001776 ) ) ;
#6626 = ORIENTED_EDGE ( 'NONE', *, *, #6196, .F. ) ;
#6627 = CARTESIAN_POINT ( 'NONE',  ( 0.02993401039713689329, -2.688325911136451474, 2.343682934607763890 ) ) ;
#6628 = DIRECTION ( 'NONE',  ( 0.000000000000000000, 1.297468594113506001E-30, 1.000000000000000000 ) ) ;
#6629 = FACE_OUTER_BOUND ( 'NONE', #1572, .T. ) ;
#6630 = CARTESIAN_POINT ( 'NONE',  ( 3.958484000408295955, -2.327740518749134679, 2.968235154689755628 ) ) ;
#6631 = ORIENTED_EDGE ( 'NONE', *, *, #6663, .F. ) ;
#6632 = ADVANCED_FACE ( 'NONE', ( #1902 ), #51, .T. ) ;
#6634 = ORIENTED_EDGE ( 'NONE', *, *, #19473, .T. ) ;
#6633 = VERTEX_POINT ( 'NONE', #19920 ) ;
#6635 = EDGE_CURVE ( 'NONE', #7856, #13205, #17807, .T. ) ;
#6636 = EDGE_LOOP ( 'NONE', ( #2061, #14459, #4024, #14560 ) ) ;
#6637 = VECTOR ( 'NONE', #20818, 1000.000000000000000 ) ;
#6638 = VERTEX_POINT ( 'NONE', #8865 ) ;
#6639 = B_SPLINE_CURVE_WITH_KNOTS ( 'NONE', 3,
 ( #5317, #16006, #3769, #3326, #21328, #15884, #3437, #1780 ),
 .UNSPECIFIED., .F., .F.,
 ( 4, 2, 2, 4 ),
 ( 0.000000000000000000, 0.0006592848877641304360, 0.001318569775528260872, 0.002637139551056521744 ),
 .UNSPECIFIED. ) ;
#6640 = ORIENTED_EDGE ( 'NONE', *, *, #11484, .T. ) ;
#6641 = VECTOR ( 'NONE', #7338, 1000.000000000000000 ) ;
#6642 = ORIENTED_EDGE ( 'NONE', *, *, #19743, .T. ) ;
#6643 = FACE_OUTER_BOUND ( 'NONE', #866, .T. ) ;
#6644 = ADVANCED_FACE ( 'NONE', ( #19801 ), #9087, .F. ) ;
#6645 = B_SPLINE_CURVE_WITH_KNOTS ( 'NONE', 3,
 ( #10239, #8368, #14250, #17413, #1200, #6838, #17529, #19537, #3202, #14010, #4834, #19187, #8487, #3428, #15646, #3075 ),
 .UNSPECIFIED., .F., .F.,
 ( 4, 3, 3, 3, 3, 4 ),
 ( -2.111273352579606344E-06, 0.000000000000000000, 3.519286887794061597E-05, 7.191842652068370593E-05, 0.0001049868727093651019, 0.0001382836236822192633 ),
 .UNSPECIFIED. ) ;
#6646 = ADVANCED_FACE ( 'NONE', ( #3788 ), #17183, .T. ) ;
#6647 = AXIS2_PLACEMENT_3D ( 'NONE', #11303, #5567, #9207 ) ;
#6648 = CARTESIAN_POINT ( 'NONE',  ( 6.000000000291855429, 2.999999999003851503, -3.449999999999997957 ) ) ;
#6649 = EDGE_LOOP ( 'NONE', ( #1831, #17391, #8146, #10883 ) ) ;
#6650 = CARTESIAN_POINT ( 'NONE',  ( -66.55000000000046612, 3.200000000000056577, -1.999999999999974021 ) ) ;
#6651 = CARTESIAN_POINT ( 'NONE',  ( 119.5756419024615838, -11.00000000000006573, -6.000000000000116351 ) ) ;
#6652 = DIRECTION ( 'NONE',  ( 1.000000000000000000, -2.168404344971005170E-16, 1.203141491611682442E-30 ) ) ;
#6653 = LINE ( 'NONE', #8306, #10085 ) ;
#6654 = FACE_OUTER_BOUND ( 'NONE', #6669, .T. ) ;
#6655 = CARTESIAN_POINT ( 'NONE',  ( 0.000000000000000000, -1.750000000000025757, 4.749999999999973355 ) ) ;
#6656 = DIRECTION ( 'NONE',  ( -0.8660254037844348218, 0.5000000000000066613, 0.000000000000000000 ) ) ;
#6657 = DIRECTION ( 'NONE',  ( -5.916456789157588541E-31, 3.382522293539642681E-32, 1.000000000000000000 ) ) ;
#6658 = DIRECTION ( 'NONE',  ( 0.8660254037844387076, 2.858508811740733972E-17, 0.4999999999999998890 ) ) ;
#6659 = ADVANCED_FACE ( 'NONE', ( #10953, #165 ), #19688, .F. ) ;
#6660 = TOROIDAL_SURFACE ( 'NONE', #6301, 4.500000000000002665, 0.5000000000000000000 ) ;
#6661 = ORIENTED_EDGE ( 'NONE', *, *, #19168, .F. ) ;
#6662 = EDGE_CURVE ( 'NONE', #278, #23028, #6690, .T. ) ;
#6663 = EDGE_CURVE ( 'NONE', #9737, #22680, #8984, .T. ) ;
#6664 =( GEOMETRIC_REPRESENTATION_CONTEXT ( 3 ) GLOBAL_UNCERTAINTY_ASSIGNED_CONTEXT ( ( #18971 ) ) GLOBAL_UNIT_ASSIGNED_CONTEXT ( ( #16343, #19411, #17647 ) ) REPRESENTATION_CONTEXT ( 'NONE', 'WORKASPACE' ) );
#6665 = CARTESIAN_POINT ( 'NONE',  ( 4.030867648404665715, 3.732851566701369528, 0.5345114293586462617 ) ) ;
#6666 = DIRECTION ( 'NONE',  ( 0.7313537016191735685, -0.6819983600624951459, 3.923113172947598083E-16 ) ) ;
#6668 = ORIENTED_EDGE ( 'NONE', *, *, #11534, .T. ) ;
#6667 = VERTEX_POINT ( 'NONE', #390 ) ;
#6669 = EDGE_LOOP ( 'NONE', ( #6038, #16378, #6696, #10030 ) ) ;
#6670 = EDGE_CURVE ( 'NONE', #22761, #178, #3903, .T. ) ;
#6671 = PRODUCT_DEFINITION_SHAPE ( 'NONE', 'NONE',  #20858 ) ;
#6672 = VECTOR ( 'NONE', #13696, 1000.000000000000000 ) ;
#6673 = ORIENTED_EDGE ( 'NONE', *, *, #15570, .F. ) ;
#6674 = DIRECTION ( 'NONE',  ( 0.000000000000000000, 0.000000000000000000, -1.000000000000000000 ) ) ;
#6675 = CYLINDRICAL_SURFACE ( 'NONE', #8035, 0.5000000000000016653 ) ;
#6676 =( BOUNDED_SURFACE ( )  B_SPLINE_SURFACE ( 3, 2, ( 
 ( #11616, #8100, #15612 ),
 ( #7980, #4685, #19147 ),
 ( #22567, #15151, #18806 ),
 ( #6684, #10099, #13628 ),
 ( #9863, #19257, #22343 ),
 ( #6225, #11858, #18926 ),
 ( #21041, #4902, #9753 ),
 ( #2679, #4557, #16904 ) ),
 .UNSPECIFIED., .F., .F., .T. ) 
 B_SPLINE_SURFACE_WITH_KNOTS ( ( 4, 2, 2, 4 ),
 ( 3, 3 ),
 ( 1.409462824231155764E-18, 0.0006647103312235273353, 0.001329420662447053370, 0.002658841324894105438 ),
 ( 0.000000000000000000, 1.000000000000000000 ),
 .UNSPECIFIED. ) 
 GEOMETRIC_REPRESENTATION_ITEM ( )  RATIONAL_B_SPLINE_SURFACE ( (
 ( 1.000000000000000000, 0.7071067811865475727, 1.000000000000000000),
 ( 1.000000000000000000, 0.7467694970717694281, 1.000000000000000000),
 ( 1.000000000000000000, 0.7847899295834248612, 1.000000000000000000),
 ( 1.000000000000000000, 0.8553546080404790253, 1.000000000000000000),
 ( 1.000000000000000000, 0.8874277420076976952, 1.000000000000000000),
 ( 1.000000000000000000, 0.9672515829044651126, 1.000000000000000000),
 ( 1.000000000000000000, 0.9993132011618868216, 1.000000000000000000),
 ( 1.000000000000000000, 0.9999716904336592993, 1.000000000000000000) ) ) 
 REPRESENTATION_ITEM ( '' )  SURFACE ( )  );
#6677 = ORIENTED_EDGE ( 'NONE', *, *, #8005, .F. ) ;
#6678 = ADVANCED_FACE ( 'NONE', ( #5224 ), #8183, .T. ) ;
#6679 = AXIS2_PLACEMENT_3D ( 'NONE', #18686, #2573, #9758 ) ;
#6680 = CARTESIAN_POINT ( 'NONE',  ( 2.742413778650726108, 1.325747111984056037, 4.749999999999997335 ) ) ;
#6681 = DIRECTION ( 'NONE',  ( -9.121204216617949000E-31, -1.000000000000000000, 6.982962677686261977E-15 ) ) ;
#6682 = AXIS2_PLACEMENT_3D ( 'NONE', #5571, #20146, #166 ) ;
#6683 = CARTESIAN_POINT ( 'NONE',  ( 42.00000000000014921, 11.00000000000000000, -12.50000000000005329 ) ) ;
#6684 = CARTESIAN_POINT ( 'NONE',  ( -5.273209981528717449, 36.26961333663339815, -18.92339500386973938 ) ) ;
#6685 = CARTESIAN_POINT ( 'NONE',  ( 4.086376042167580103, 4.082715877136795513, -0.07147133206921667259 ) ) ;
#6686 = AXIS2_PLACEMENT_3D ( 'NONE', #23188, #12339, #1533 ) ;
#6687 = CARTESIAN_POINT ( 'NONE',  ( -8.954763739086818219, -0.4999999999999885092, 6.678571428571394186 ) ) ;
#6688 = VECTOR ( 'NONE', #8654, 1000.000000000000000 ) ;
#6689 = FACE_OUTER_BOUND ( 'NONE', #10341, .T. ) ;
#6690 = CIRCLE ( 'NONE', #7068, 2.550000000000010481 ) ;
#6691 = DIRECTION ( 'NONE',  ( -2.220446049250313081E-16, 1.000000000000000000, -7.025792437124636392E-31 ) ) ;
#6692 = CARTESIAN_POINT ( 'NONE',  ( -42.54314575050799618, 5.299999999999998934, 8.000000000000035527 ) ) ;
#6693 = CARTESIAN_POINT ( 'NONE',  ( 24.74999999999997513, 0.000000000000000000, -2.081668171172168513E-14 ) ) ;
#6694 = FACE_OUTER_BOUND ( 'NONE', #17932, .T. ) ;
#6695 = DIRECTION ( 'NONE',  ( 1.000000000000000000, 0.000000000000000000, 0.000000000000000000 ) ) ;
#6696 = ORIENTED_EDGE ( 'NONE', *, *, #15570, .T. ) ;
#6697 = ORIENTED_EDGE ( 'NONE', *, *, #6289, .T. ) ;
#6698 = EDGE_CURVE ( 'NONE', #11731, #11726, #7779, .T. ) ;
#6699 = DIRECTION ( 'NONE',  ( 1.454462294001240516E-30, 1.000000000000000000, 0.000000000000000000 ) ) ;
#6700 = VECTOR ( 'NONE', #2961, 1000.000000000000000 ) ;
#6702 = ORIENTED_EDGE ( 'NONE', *, *, #12164, .F. ) ;
#6701 = ORIENTED_EDGE ( 'NONE', *, *, #10902, .F. ) ;
#6703 = CONICAL_SURFACE ( 'NONE', #20983, 4.000000000000022204, 0.8911886515913840512 ) ;
#6704 = VECTOR ( 'NONE', #3702, 1000.000000000000000 ) ;
#6705 = B_SPLINE_CURVE_WITH_KNOTS ( 'NONE', 3,
 ( #11274, #9754, #11042, #18231, #582, #815 ),
 .UNSPECIFIED., .F., .F.,
 ( 4, 2, 4 ),
 ( -3.640115492440753560E-06, 0.0002066546034006306394, 0.0004169493222937020434 ),
 .UNSPECIFIED. ) ;
#6706 = CARTESIAN_POINT ( 'NONE',  ( -55.05572809000126711, 3.200000000000022382, -7.500000000000034639 ) ) ;
#6707 = ORIENTED_EDGE ( 'NONE', *, *, #23182, .F. ) ;
#6708 = EDGE_CURVE ( 'NONE', #20837, #7256, #22828, .T. ) ;
#6709 = CARTESIAN_POINT ( 'NONE',  ( -12.85000000000004228, -0.5000000000000004441, -6.249999999999977796 ) ) ;
#6710 = CARTESIAN_POINT ( 'NONE',  ( -6.959810536856680940, 36.00015702695179698, -26.48940942388196618 ) ) ;
#6711 = ORIENTED_EDGE ( 'NONE', *, *, #10523, .T. ) ;
#6712 = FACE_OUTER_BOUND ( 'NONE', #19626, .T. ) ;
#6713 = CARTESIAN_POINT ( 'NONE',  ( -95.70000000000071338, 0.5000000000000073275, 1.000000000000070166 ) ) ;
#6714 = FACE_OUTER_BOUND ( 'NONE', #4026, .T. ) ;
#6715 = DIRECTION ( 'NONE',  ( 1.281898970984144184E-30, 1.000000000000000000, 6.938893903907263876E-15 ) ) ;
#6716 = MECHANICAL_DESIGN_GEOMETRIC_PRESENTATION_REPRESENTATION (  '', ( #5203 ), #5965 ) ;
#6717 = FACE_OUTER_BOUND ( 'NONE', #18842, .T. ) ;
#6718 = CYLINDRICAL_SURFACE ( 'NONE', #9504, 0.5000000000000016653 ) ;
#6719 = CIRCLE ( 'NONE', #5604, 6.000000000000036415 ) ;
#6720 = DIRECTION ( 'NONE',  ( -1.000000000000000000, 1.550910762415502399E-16, 0.000000000000000000 ) ) ;
#6721 = DIRECTION ( 'NONE',  ( 3.032184104443272185E-30, 1.000000000000000000, -7.395570986447005381E-32 ) ) ;
#6722 = CIRCLE ( 'NONE', #15728, 0.4999999999999990563 ) ;
#6723 = CYLINDRICAL_SURFACE ( 'NONE', #2943, 2.550000000000010481 ) ;
#6724 = VERTEX_POINT ( 'NONE', #17059 ) ;
#6725 = DIRECTION ( 'NONE',  ( 0.000000000000000000, -1.000000000000000000, 2.775557561562891351E-17 ) ) ;
#6727 = VERTEX_POINT ( 'NONE', #11425 ) ;
#6726 = ORIENTED_EDGE ( 'NONE', *, *, #4262, .F. ) ;
#6728 = VERTEX_POINT ( 'NONE', #620 ) ;
#6730 = ORIENTED_EDGE ( 'NONE', *, *, #3786, .F. ) ;
#6729 = ORIENTED_EDGE ( 'NONE', *, *, #9603, .T. ) ;
#6731 = ORIENTED_EDGE ( 'NONE', *, *, #1058, .T. ) ;
#6732 = CARTESIAN_POINT ( 'NONE',  ( 0.000000000000000000, 0.000000000000000000, -5.600000000000000533 ) ) ;
#6733 = CARTESIAN_POINT ( 'NONE',  ( 12.84999999999997300, -1.500000000000001332, 6.250000000000005329 ) ) ;
#6734 = CYLINDRICAL_SURFACE ( 'NONE', #9532, 2.550000000000000711 ) ;
#6735 = COLOUR_RGB ( '', 0.08235294, 0.09019608, 0.10196078) ;
#6736 = DIRECTION ( 'NONE',  ( 0.9396926207859150892, -1.094182011322127520E-15, -0.3420201433256501722 ) ) ;
#6737 = CARTESIAN_POINT ( 'NONE',  ( -7.000000000000006217, -0.9711575687493188003, 9.522727272727280479 ) ) ;
#6738 = CARTESIAN_POINT ( 'NONE',  ( -8.181569977154534712, -2.135203747983297262, 7.340676138759476110 ) ) ;
#6739 = DIRECTION ( 'NONE',  ( -4.190823558986625216E-31, 1.000000000000000000, -4.190823558986625216E-31 ) ) ;
#6740 = DIRECTION ( 'NONE',  ( -3.070652698126927723E-17, -1.000000000000000000, 4.167305704548413124E-17 ) ) ;
#6741 = CIRCLE ( 'NONE', #17257, 5.999999999999998224 ) ;
#6742 = CARTESIAN_POINT ( 'NONE',  ( 3.961557105775642462, -1.423285172353593087, 3.499999999999995559 ) ) ;
#6743 = CARTESIAN_POINT ( 'NONE',  ( -3.499999999708153453, 2.999999999003851503, -25.50000000000000000 ) ) ;
#6744 = COLOUR_RGB ( '', 0.08235294, 0.09019608, 0.10196078) ;
#6745 = EDGE_CURVE ( 'NONE', #20589, #18641, #15669, .T. ) ;
#6746 = CARTESIAN_POINT ( 'NONE',  ( -42.54314575050796776, 7.499999999999992895, -8.000000000000035527 ) ) ;
#6747 = CARTESIAN_POINT ( 'NONE',  ( 119.5756419024616406, -6.500000000000005329, 6.500000000000151879 ) ) ;
#6748 = CARTESIAN_POINT ( 'NONE',  ( 66.26395429947838522, 0.000000000000000000, -6.499999999999859668 ) ) ;
#6749 = DIRECTION ( 'NONE',  ( 1.733449886265891589E-32, -4.190823558986610327E-31, 1.000000000000000000 ) ) ;
#6750 = ORIENTED_EDGE ( 'NONE', *, *, #7539, .F. ) ;
#6751 = FILL_AREA_STYLE ('',( #10742 ) ) ;
#6753 = ORIENTED_EDGE ( 'NONE', *, *, #13810, .T. ) ;
#6752 = VERTEX_POINT ( 'NONE', #16586 ) ;
#6754 = EDGE_LOOP ( 'NONE', ( #14079, #6088, #8173, #9163 ) ) ;
#6755 = ORIENTED_EDGE ( 'NONE', *, *, #22468, .F. ) ;
#6756 = VECTOR ( 'NONE', #2279, 1000.000000000000000 ) ;
#6757 = EDGE_LOOP ( 'NONE', ( #7768, #6016, #20333, #4861 ) ) ;
#6758 = ORIENTED_EDGE ( 'NONE', *, *, #18052, .F. ) ;
#6759 = DIRECTION ( 'NONE',  ( 5.551115123561405253E-17, 1.000000000000000000, 2.256980353643891447E-27 ) ) ;
#6760 = B_SPLINE_CURVE_WITH_KNOTS ( 'NONE', 3,
 ( #23190, #14346, #10584, #17765, #10349, #21193 ),
 .UNSPECIFIED., .F., .F.,
 ( 4, 2, 4 ),
 ( 0.004120275011746847918, 0.005288420935197131814, 0.006456566858647415710 ),
 .UNSPECIFIED. ) ;
#6761 = CARTESIAN_POINT ( 'NONE',  ( 4.071447262713884463, -2.020725942163688504, 3.499999999999997780 ) ) ;
#6762 = ORIENTED_EDGE ( 'NONE', *, *, #5386, .T. ) ;
#6763 = CARTESIAN_POINT ( 'NONE',  ( -47.82842712474658242, 4.371572875253824542, -7.500000000000007105 ) ) ;
#6764 = CARTESIAN_POINT ( 'NONE',  ( 4.211140560182194292, -2.431303136016568889, -3.745885042887441063 ) ) ;
#6765 = ADVANCED_FACE ( 'NONE', ( #16821 ), #4355, .F. ) ;
#6766 = FACE_OUTER_BOUND ( 'NONE', #1101, .T. ) ;
#6767 = DIRECTION ( 'NONE',  ( -5.598259082250079541E-17, 1.000000000000000000, -6.162975822039171151E-32 ) ) ;
#6768 = DIRECTION ( 'NONE',  ( 5.551115123125782702E-16, 1.201780285297635172E-31, -1.000000000000000000 ) ) ;
#6769 = DIRECTION ( 'NONE',  ( -0.8191520442889964615, 1.029921702463447212E-15, -0.5735764363510394981 ) ) ;
#6770 = CARTESIAN_POINT ( 'NONE',  ( 22.49999999999996092, 2.000000000000043521, -17.75000000000001066 ) ) ;
#6771 = EDGE_CURVE ( 'NONE', #16034, #15424, #20580, .T. ) ;
#6772 = DIRECTION ( 'NONE',  ( -1.000000000000000000, 1.700709290173333260E-16, 0.000000000000000000 ) ) ;
#6773 = VECTOR ( 'NONE', #4227, 1000.000000000000000 ) ;
#6774 = CARTESIAN_POINT ( 'NONE',  ( -6.979783269036462734, 14.00008466144083030, -18.59869175759557791 ) ) ;
#6775 = B_SPLINE_CURVE_WITH_KNOTS ( 'NONE', 3,
 ( #12691, #7179, #5759, #5527, #21535, #14339, #16328, #11037, #16439, #19760, #2219, #5419, #1978, #21649 ),
 .UNSPECIFIED., .F., .F.,
 ( 4, 2, 2, 2, 2, 2, 4 ),
 ( 0.000000000000000000, 0.0008860460682957670793, 0.001772092136591534159, 0.002215115170739416234, 0.002658138204887298961, 0.003101161239035180820, 0.003544184273183063547 ),
 .UNSPECIFIED. ) ;
#6776 = DIRECTION ( 'NONE',  ( 1.858632295689435609E-16, 1.000000000000000000, -0.000000000000000000 ) ) ;
#6777 = CARTESIAN_POINT ( 'NONE',  ( 8.200527591913237657, -12.43937801162580925, 7.318116290495840559 ) ) ;
#6778 = ORIENTED_EDGE ( 'NONE', *, *, #21008, .F. ) ;
#6779 = EDGE_CURVE ( 'NONE', #1430, #14170, #2258, .T. ) ;
#6780 = PRESENTATION_STYLE_ASSIGNMENT (( #19832 ) ) ;
#6781 = DIRECTION ( 'NONE',  ( -1.000000000000000000, -2.699383410053119644E-30, -3.330669073875432643E-16 ) ) ;
#6782 = CARTESIAN_POINT ( 'NONE',  ( 0.000000000000000000, 0.000000000000000000, 3.469446951953614189E-15 ) ) ;
#6783 = EDGE_CURVE ( 'NONE', #10966, #19955, #15061, .T. ) ;
#6785 = ORIENTED_EDGE ( 'NONE', *, *, #1723, .F. ) ;
#6784 = ORIENTED_EDGE ( 'NONE', *, *, #13956, .T. ) ;
#6786 = EDGE_CURVE ( 'NONE', #19782, #17658, #2486, .T. ) ;
#6787 = ORIENTED_EDGE ( 'NONE', *, *, #1501, .F. ) ;
#6788 = ORIENTED_EDGE ( 'NONE', *, *, #20906, .T. ) ;
#6789 = DIRECTION ( 'NONE',  ( -1.000000000000000000, -3.469446951953617344E-15, 0.000000000000000000 ) ) ;
#6790 = CARTESIAN_POINT ( 'NONE',  ( -6.746326818733313857, 0.5000000000001045830, 27.22340457528590818 ) ) ;
#6791 = VECTOR ( 'NONE', #2101, 1000.000000000000000 ) ;
#6792 = CARTESIAN_POINT ( 'NONE',  ( -12.84999999999999964, -14.00000000000003020, 5.750000000000032863 ) ) ;
#6793 = CARTESIAN_POINT ( 'NONE',  ( 27.99999999999991473, 2.500000000000009326, 0.000000000000000000 ) ) ;
#6794 = EDGE_CURVE ( 'NONE', #18297, #7463, #14199, .T. ) ;
#6795 = DIRECTION ( 'NONE',  ( 5.551115123125796261E-17, -2.869019762633796499E-16, -1.000000000000000000 ) ) ;
#6796 = EDGE_CURVE ( 'NONE', #2883, #14796, #22020, .T. ) ;
#6797 = DIRECTION ( 'NONE',  ( -8.438582421954109416E-32, 0.000000000000000000, -1.000000000000000000 ) ) ;
#6798 = DIRECTION ( 'NONE',  ( 1.000000000000000000, 2.220446049250313081E-16, -3.656342123407315983E-48 ) ) ;
#6799 = CARTESIAN_POINT ( 'NONE',  ( 2.775557561562891351E-14, 8.000000000000003553, -12.50000000000001066 ) ) ;
#6800 = DIRECTION ( 'NONE',  ( 8.438582421954110511E-32, 0.000000000000000000, -1.000000000000000000 ) ) ;
#6801 = CARTESIAN_POINT ( 'NONE',  ( -4.580847626785981674, -1.750000000000056399, -1.565739168675184478 ) ) ;
#6802 = DIRECTION ( 'NONE',  ( 1.000000000000000000, -4.437342591868175641E-31, 3.330669073875457788E-16 ) ) ;
#6803 = DIRECTION ( 'NONE',  ( -1.000000000000000000, 1.550910762415496482E-16, -6.938893903907184004E-16 ) ) ;
#6804 = CARTESIAN_POINT ( 'NONE',  ( 4.630153689607049650, 6.577590292450094690E-16, 5.371010071662835728 ) ) ;
#6805 = EDGE_CURVE ( 'NONE', #9710, #11691, #16424, .T. ) ;
#6806 = LINE ( 'NONE', #13974, #13013 ) ;
#6807 = EDGE_CURVE ( 'NONE', #18911, #9721, #18487, .T. ) ;
#6808 = EDGE_CURVE ( 'NONE', #14530, #9714, #16058, .T. ) ;
#6809 = CARTESIAN_POINT ( 'NONE',  ( -2.687328764639671075, 3.067272167851270215, -0.05923475698270320999 ) ) ;
#6811 = CIRCLE ( 'NONE', #3435, 0.4999999999999978351 ) ;
#6810 = DIRECTION ( 'NONE',  ( -7.860214984770699307E-18, 1.409037165336591006E-16, 1.000000000000000000 ) ) ;
#6812 = AXIS2_PLACEMENT_3D ( 'NONE', #8309, #16761, #20437 ) ;
#6813 = ORIENTED_EDGE ( 'NONE', *, *, #18447, .F. ) ;
#6814 = ADVANCED_FACE ( 'NONE', ( #13083 ), #22088, .T. ) ;
#6815 = VERTEX_POINT ( 'NONE', #2603 ) ;
#6816 = DIRECTION ( 'NONE',  ( -1.066723072283233324E-26, 0.000000000000000000, -1.000000000000000000 ) ) ;
#6818 = ORIENTED_EDGE ( 'NONE', *, *, #11577, .F. ) ;
#6817 = ORIENTED_EDGE ( 'NONE', *, *, #4481, .F. ) ;
#6819 = CARTESIAN_POINT ( 'NONE',  ( -7.499999999999992895, -5.999999999999981348, 11.74999999999998224 ) ) ;
#6820 = ORIENTED_EDGE ( 'NONE', *, *, #18576, .T. ) ;
#6821 = CYLINDRICAL_SURFACE ( 'NONE', #9985, 2.999999999999995559 ) ;
#6822 = CARTESIAN_POINT ( 'NONE',  ( 0.000000000000000000, 0.000000000000000000, 0.000000000000000000 ) ) ;
#6823 = CARTESIAN_POINT ( 'NONE',  ( -3.499999999708153453, 35.49999999900384751, -19.00000000000000355 ) ) ;
#6824 = EDGE_CURVE ( 'NONE', #20968, #17687, #11928, .T. ) ;
#6825 = VERTEX_POINT ( 'NONE', #4017 ) ;
#6826 = CARTESIAN_POINT ( 'NONE',  ( 2.918498775983380256E-10, 6.999999999003851947, -19.00000000000000355 ) ) ;
#6827 = TOROIDAL_SURFACE ( 'NONE', #22987, 3.299999999999999822, 0.5000000000000000000 ) ;
#6828 = VECTOR ( 'NONE', #450, 1000.000000000000000 ) ;
#6829 = CARTESIAN_POINT ( 'NONE',  ( 3.534277608972077545, -1.672424706883764989, 3.378451613207321014 ) ) ;
#6830 = DIRECTION ( 'NONE',  ( -1.000000000000000000, -4.252453317207022018E-31, 5.551115123125818447E-17 ) ) ;
#6831 = FACE_OUTER_BOUND ( 'NONE', #3114, .T. ) ;
#6832 = CARTESIAN_POINT ( 'NONE',  ( 0.000000000000000000, 1.750000000000001554, 0.000000000000000000 ) ) ;
#6833 = CARTESIAN_POINT ( 'NONE',  ( 4.101954839143034270, -2.368264730582960720, -3.681130640444259861 ) ) ;
#6834 = CARTESIAN_POINT ( 'NONE',  ( -7.000000000000033751, -11.35410196624970780, 9.250000000000063949 ) ) ;
#6835 = ADVANCED_FACE ( 'NONE', ( #4241 ), #9782, .T. ) ;
#6836 = CARTESIAN_POINT ( 'NONE',  ( 77.42435809754140053, -10.99999999999981526, -6.499999999999999112 ) ) ;
#6837 = CARTESIAN_POINT ( 'NONE',  ( -50.65685424949274562, -0.5000000000001045830, 8.000000000000062172 ) ) ;
#6838 = CARTESIAN_POINT ( 'NONE',  ( 4.165266963751727225, -4.099263933823985795, 2.410680203327883803E-15 ) ) ;
#6839 = ORIENTED_EDGE ( 'NONE', *, *, #7772, .F. ) ;
#6840 = CARTESIAN_POINT ( 'NONE',  ( -25.13934240061088232, 60.78549366357397332, 34.16570243528389028 ) ) ;
#6841 = AXIS2_PLACEMENT_3D ( 'NONE', #15952, #12899, #16409 ) ;
#6843 = ORIENTED_EDGE ( 'NONE', *, *, #18170, .T. ) ;
#6842 = ORIENTED_EDGE ( 'NONE', *, *, #20032, .F. ) ;
#6844 = ORIENTED_EDGE ( 'NONE', *, *, #10877, .F. ) ;
#6846 = ORIENTED_EDGE ( 'NONE', *, *, #5480, .F. ) ;
#6845 = ORIENTED_EDGE ( 'NONE', *, *, #11582, .T. ) ;
#6847 = DIRECTION ( 'NONE',  ( 0.000000000000000000, 0.000000000000000000, 1.000000000000000000 ) ) ;
#6848 = CARTESIAN_POINT ( 'NONE',  ( -4.197393957002394593, -7.172049766556752605E-14, -3.503767560748959120 ) ) ;
#6849 = LINE ( 'NONE', #1553, #12909 ) ;
#6850 = CARTESIAN_POINT ( 'NONE',  ( -12.85000000000002807, -12.00000000000002842, 6.250000000000019540 ) ) ;
#6851 = CARTESIAN_POINT ( 'NONE',  ( 54.42435809754118736, 2.999999999999947153, -6.499999999999922728 ) ) ;
#6852 = DIRECTION ( 'NONE',  ( 0.000000000000000000, 0.000000000000000000, 1.000000000000000000 ) ) ;
#6853 =( BOUNDED_SURFACE ( )  B_SPLINE_SURFACE ( 3, 2, ( 
 ( #23173, #5281, #22090 ),
 ( #16537, #13032, #7508 ),
 ( #4304, #20324, #14671 ),
 ( #13261, #570, #21978 ),
 ( #20096, #443, #9496 ),
 ( #2437, #2316, #7620 ) ),
 .UNSPECIFIED., .F., .F., .T. ) 
 B_SPLINE_SURFACE_WITH_KNOTS ( ( 4, 2, 4 ),
 ( 3, 3 ),
 ( 0.01652267773200354062, 0.01858309280828997906, 0.02064350788457642097 ),
 ( 0.000000000000000000, 1.000000000000000000 ),
 .UNSPECIFIED. ) 
 GEOMETRIC_REPRESENTATION_ITEM ( )  RATIONAL_B_SPLINE_SURFACE ( (
 ( 1.000000000000000000, 0.8047780975688292315, 1.000000000000000000),
 ( 1.000000000000000000, 0.8123789546323675337, 1.000000000000000000),
 ( 1.000000000000000000, 0.8190677982989954531, 1.000000000000000000),
 ( 1.000000000000000000, 0.8192346069550978660, 1.000000000000000000),
 ( 1.000000000000000000, 0.8126126759769800589, 1.000000000000000000),
 ( 1.000000000000000000, 0.8047712639312011307, 1.000000000000000000) ) ) 
 REPRESENTATION_ITEM ( '' )  SURFACE ( )  );
#6854 = FACE_OUTER_BOUND ( 'NONE', #5343, .T. ) ;
#6855 = ADVANCED_FACE ( 'NONE', ( #22601 ), #10020, .T. ) ;
#6856 = DIRECTION ( 'NONE',  ( 1.550910762415566494E-16, 1.000000000000000000, -8.135128085091684243E-31 ) ) ;
#6857 = CARTESIAN_POINT ( 'NONE',  ( -95.20000000000061391, -0.5000000000000975886, 1.000000000000028644 ) ) ;
#6858 = CIRCLE ( 'NONE', #14762, 4.000000000000023981 ) ;
#6859 = DIRECTION ( 'NONE',  ( 0.000000000000000000, 0.000000000000000000, 1.000000000000000000 ) ) ;
#6860 = VECTOR ( 'NONE', #21272, 1000.000000000000000 ) ;
#6861 = DIRECTION ( 'NONE',  ( -1.232595164407830946E-32, 1.000000000000000000, -6.938893903907214967E-15 ) ) ;
#6862 = ADVANCED_FACE ( 'NONE', ( #15300 ), #6723, .F. ) ;
#6863 = AXIS2_PLACEMENT_3D ( 'NONE', #17343, #16878, #3010 ) ;
#6864 = CIRCLE ( 'NONE', #1980, 0.5000000000000028866 ) ;
#6865 = CARTESIAN_POINT ( 'NONE',  ( 4.630153689607046985, -1.834136773469866309E-30, -5.371010071662817076 ) ) ;
#6866 = CARTESIAN_POINT ( 'NONE',  ( -7.629227790279501598, -12.04719844907614146, 8.369856247450657705 ) ) ;
#6867 = CARTESIAN_POINT ( 'NONE',  ( -64.00000000000045475, 2.700000000000056577, -1.999999999999974021 ) ) ;
#6868 = DIRECTION ( 'NONE',  ( 9.470910429910671536E-17, 0.000000000000000000, -1.000000000000000000 ) ) ;
#6869 = PRODUCT ( 'Bracket washer', 'Bracket washer', '', ( #14252 ) ) ;
#6870 = EDGE_CURVE ( 'NONE', #5817, #13979, #16817, .T. ) ;
#6871 = ORIENTED_EDGE ( 'NONE', *, *, #18748, .F. ) ;
#6872 = STYLED_ITEM ( 'NONE', ( #21908 ), #5542 ) ;
#6873 = SURFACE_STYLE_FILL_AREA ( #6751 ) ;
#6875 = ORIENTED_EDGE ( 'NONE', *, *, #183, .F. ) ;
#6874 = VERTEX_POINT ( 'NONE', #6837 ) ;
#6876 = ORIENTED_EDGE ( 'NONE', *, *, #4360, .T. ) ;
#6877 = ORIENTED_EDGE ( 'NONE', *, *, #591, .F. ) ;
#6878 = AXIS2_PLACEMENT_3D ( 'NONE', #18829, #21070, #4471 ) ;
#6879 = VERTEX_POINT ( 'NONE', #22493 ) ;
#6880 = CIRCLE ( 'NONE', #13646, 0.5000000000000017764 ) ;
#6881 = AXIS2_PLACEMENT_3D ( 'NONE', #6284, #14980, #9696 ) ;
#6882 = AXIS2_PLACEMENT_3D ( 'NONE', #36, #8850, #21217 ) ;
#6883 = EDGE_LOOP ( 'NONE', ( #16033, #2971, #8847, #16721 ) ) ;
#6884 = DIRECTION ( 'NONE',  ( -8.381647117973248681E-31, 0.5000000000000012212, -0.8660254037844379305 ) ) ;
#6885 = CARTESIAN_POINT ( 'NONE',  ( 42.50000000000014921, 2.999999999999999112, -0.4999999999999726885 ) ) ;
#6886 = ORIENTED_EDGE ( 'NONE', *, *, #13870, .F. ) ;
#6887 = DIRECTION ( 'NONE',  ( 1.000000000000000000, 2.220446049250300755E-16, 2.081668171172155103E-15 ) ) ;
#6888 = CARTESIAN_POINT ( 'NONE',  ( 1.747541505913256188, -3.837784562140331257, -3.503702292528931395 ) ) ;
#6889 = CYLINDRICAL_SURFACE ( 'NONE', #9493, 0.5000000000000017764 ) ;
#6890 = DIRECTION ( 'NONE',  ( -1.000000000000000000, 0.000000000000000000, 0.000000000000000000 ) ) ;
#6891 = CARTESIAN_POINT ( 'NONE',  ( -7.523653856849436217, -1.079621694564730783, 8.801128846369456582 ) ) ;
#6892 = DIRECTION ( 'NONE',  ( -5.551115123561405253E-17, -1.000000000000000000, -2.256980353643891447E-27 ) ) ;
#6893 = FACE_OUTER_BOUND ( 'NONE', #22141, .T. ) ;
#6894 = PLANE ( 'NONE',  #3436 ) ;
#6895 = CARTESIAN_POINT ( 'NONE',  ( -45.56568542494948559, -2.108831175456959972, 8.000000000000062172 ) ) ;
#6896 = CIRCLE ( 'NONE', #14022, 2.549999999999998490 ) ;
#6897 = VECTOR ( 'NONE', #20697, 999.9999999999998863 ) ;
#6898 = CARTESIAN_POINT ( 'NONE',  ( 6.000000000291855429, -0.5000000009961480529, -41.55000000000000426 ) ) ;
#6899 = AXIS2_PLACEMENT_3D ( 'NONE', #16733, #16848, #18627 ) ;
#6900 = CYLINDRICAL_SURFACE ( 'NONE', #6265, 0.4999999999999987232 ) ;
#6901 = CIRCLE ( 'NONE', #23058, 4.582731094065982447 ) ;
#6902 = ORIENTED_EDGE ( 'NONE', *, *, #21008, .T. ) ;
#6903 = AXIS2_PLACEMENT_3D ( 'NONE', #2119, #21893, #9306 ) ;
#6904 = MECHANICAL_DESIGN_GEOMETRIC_PRESENTATION_REPRESENTATION (  '', ( #3878 ), #15150 ) ;
#6905 = CARTESIAN_POINT ( 'NONE',  ( 4.211140560182139225, 2.431303136016540911, -3.745885042887430405 ) ) ;
#6906 = DIRECTION ( 'NONE',  ( -1.000000000000000000, 1.577021341797084002E-16, -9.777532319141921008E-15 ) ) ;
#6908 = EDGE_LOOP ( 'NONE', ( #5613, #20840, #4979, #16176 ) ) ;
#6907 = ORIENTED_EDGE ( 'NONE', *, *, #9301, .F. ) ;
#6909 = PRODUCT_RELATED_PRODUCT_CATEGORY ( 'part', '', ( #13808 ) ) ;
#6910 = EDGE_LOOP ( 'NONE', ( #20100, #5109, #246, #3464 ) ) ;
#6911 = VERTEX_POINT ( 'NONE', #21077 ) ;
#6912 = ORIENTED_EDGE ( 'NONE', *, *, #20155, .T. ) ;
#6913 = EDGE_CURVE ( 'NONE', #13336, #18554, #4942, .T. ) ;
#6914 = CARTESIAN_POINT ( 'NONE',  ( -50.65685424949267457, 7.200000000000018829, -7.500000000000034639 ) ) ;
#6915 = FACE_OUTER_BOUND ( 'NONE', #15602, .T. ) ;
#6916 = AXIS2_PLACEMENT_3D ( 'NONE', #6320, #13494, #8435 ) ;
#6917 = AXIS2_PLACEMENT_3D ( 'NONE', #11800, #1116, #18988 ) ;
#6918 = CARTESIAN_POINT ( 'NONE',  ( -3.191035955565509674, -1.584759246591024517, 3.972963596181419810 ) ) ;
#6919 = AXIS2_PLACEMENT_3D ( 'NONE', #6340, #6452, #19040 ) ;
#6920 = AXIS2_PLACEMENT_3D ( 'NONE', #17011, #2912, #15373 ) ;
#6921 = CARTESIAN_POINT ( 'NONE',  ( 36.00000000029184832, 5.999999999003851059, -16.00000000000000000 ) ) ;
#6922 = CARTESIAN_POINT ( 'NONE',  ( -45.37157287525403149, -6.828427124746218269, -7.500000000000034639 ) ) ;
#6923 = ADVANCED_FACE ( 'NONE', ( #18961 ), #15416, .T. ) ;
#6924 = DIRECTION ( 'NONE',  ( 1.000000000000000000, 4.882007496677533029E-14, 3.717264591378832268E-16 ) ) ;
#6925 = DIRECTION ( 'NONE',  ( -9.121204216617949000E-31, -1.000000000000000000, 6.982962677686261977E-15 ) ) ;
#6926 = CARTESIAN_POINT ( 'NONE',  ( -7.951003271401643424, -0.1617022081437910763, 7.659883344695618490 ) ) ;
#6927 = CYLINDRICAL_SURFACE ( 'NONE', #20130, 10.00000000000006395 ) ;
#6928 = CARTESIAN_POINT ( 'NONE',  ( 4.630153689607049650, -1.816756130622550821E-31, -5.371010071662842833 ) ) ;
#6929 = DIRECTION ( 'NONE',  ( -1.000000000000000000, 1.517883041479696593E-16, 0.000000000000000000 ) ) ;
#6930 = DIRECTION ( 'NONE',  ( 0.000000000000000000, 0.000000000000000000, -1.000000000000000000 ) ) ;
#6931 = DIRECTION ( 'NONE',  ( 0.000000000000000000, 0.000000000000000000, -1.000000000000000000 ) ) ;
#6932 = CARTESIAN_POINT ( 'NONE',  ( -1.243802165050142072, 3.900692638706738435, -3.223146290109823120 ) ) ;
#6933 = CIRCLE ( 'NONE', #9561, 6.000000000000022204 ) ;
#6934 = LINE ( 'NONE', #16081, #4076 ) ;
#6935 = CLOSED_SHELL ( 'NONE', ( #446, #4756, #22376, #15953, #7228, #931, #20064, #20071, #18879, #11164, #20097, #4781, #1622, #7752, #8694, #4197, #4285, #14995, #21613, #646, #18889, #308 ) ) ;
#6936 = AXIS2_PLACEMENT_3D ( 'NONE', #967, #4588, #4938 ) ;
#6937 = CARTESIAN_POINT ( 'NONE',  ( -1.317756351988384145, 3.857995168970181687, -0.04852650426600636085 ) ) ;
#6938 = VERTEX_POINT ( 'NONE', #6605 ) ;
#6939 = AXIS2_PLACEMENT_3D ( 'NONE', #20308, #7264, #16637 ) ;
#6940 = EDGE_CURVE ( 'NONE', #7345, #3408, #20729, .T. ) ;
#6941 = ORIENTED_EDGE ( 'NONE', *, *, #10131, .F. ) ;
#6942 = EDGE_CURVE ( 'NONE', #10886, #19955, #22102, .T. ) ;
#6943 = DIRECTION ( 'NONE',  ( -3.254448077146059901E-32, -1.000000000000000000, -6.409494854920712161E-31 ) ) ;
#6945 = ORIENTED_EDGE ( 'NONE', *, *, #10523, .F. ) ;
#6944 = VERTEX_POINT ( 'NONE', #11889 ) ;
#6946 = CARTESIAN_POINT ( 'NONE',  ( 116.5066492821802768, -7.708908342713760575, 6.500000000000151879 ) ) ;
#6947 = CARTESIAN_POINT ( 'NONE',  ( 1.999999999999953149, -3.464101615137771262, 0.000000000000000000 ) ) ;
#6948 = DIRECTION ( 'NONE',  ( 1.000000000000000000, -1.424116703980815236E-16, -2.931272055834072749E-32 ) ) ;
#6949 = CARTESIAN_POINT ( 'NONE',  ( -4.550510256924974684, 36.49999999900384751, -26.00000000000000000 ) ) ;
#6950 = AXIS2_PLACEMENT_3D ( 'NONE', #841, #6254, #4825 ) ;
#6952 = ORIENTED_EDGE ( 'NONE', *, *, #15265, .T. ) ;
#6951 = EDGE_CURVE ( 'NONE', #6327, #1919, #1320, .T. ) ;
#6953 = ADVANCED_BREP_SHAPE_REPRESENTATION ( '', ( #5542, #22115 ), #22911 ) ;
#6954 = CIRCLE ( 'NONE', #16332, 0.4999999999999990563 ) ;
#6955 = FACE_OUTER_BOUND ( 'NONE', #15070, .T. ) ;
#6956 = CARTESIAN_POINT ( 'NONE',  ( -55.25320565519140104, -3.200000000000108979, 7.500000000000047962 ) ) ;
#6957 = EDGE_CURVE ( 'NONE', #8927, #4863, #20961, .T. ) ;
#6958 = CARTESIAN_POINT ( 'NONE',  ( 0.2182387239031264026, 1.693823289467349946, -3.500000000000008438 ) ) ;
#6959 = EDGE_CURVE ( 'NONE', #22269, #1665, #13082, .T. ) ;
#6960 = CARTESIAN_POINT ( 'NONE',  ( -8.414481090081503467, -14.00000000000004263, 6.435353702847475432 ) ) ;
#6961 = CARTESIAN_POINT ( 'NONE',  ( -42.54314575050795355, 4.799999999999991829, -7.500000000000007105 ) ) ;
#6962 = CARTESIAN_POINT ( 'NONE',  ( 7.500000000000007105, -2.645898033750298417, 9.250000000000019540 ) ) ;
#6963 = CARTESIAN_POINT ( 'NONE',  ( 4.175572532730932984, 2.061029303918059608, -3.569807470274386052 ) ) ;
#6964 = CARTESIAN_POINT ( 'NONE',  ( -95.70000000000065654, -0.5000000000000975886, -2.000000000000029310 ) ) ;
#6965 = DIRECTION ( 'NONE',  ( 7.860214984770699307E-18, -1.409037165336591006E-16, -1.000000000000000000 ) ) ;
#6966 = FACE_OUTER_BOUND ( 'NONE', #20592, .T. ) ;
#6967 = EDGE_CURVE ( 'NONE', #6496, #18651, #11197, .T. ) ;
#6968 = ADVANCED_FACE ( 'NONE', ( #10357, #21202, #12225 ), #17528, .T. ) ;
#6969 = VERTEX_POINT ( 'NONE', #3654 ) ;
#6970 = EDGE_CURVE ( 'NONE', #20034, #14654, #11155, .T. ) ;
#6971 = CIRCLE ( 'NONE', #11462, 3.500000000000004441 ) ;
#6972 = ADVANCED_FACE ( 'NONE', ( #3873 ), #14590, .F. ) ;
#6973 = CARTESIAN_POINT ( 'NONE',  ( -49.56813518628801063, 78.19911141045380987, 34.16570243528392581 ) ) ;
#6974 = AXIS2_PLACEMENT_3D ( 'NONE', #4708, #17045, #10005 ) ;
#6976 = EDGE_LOOP ( 'NONE', ( #1363, #12770, #16688, #12038, #18468 ) ) ;
#6975 = ORIENTED_EDGE ( 'NONE', *, *, #1042, .T. ) ;
#6977 = EDGE_LOOP ( 'NONE', ( #15941, #2722, #22874, #6843 ) ) ;
#6979 = ORIENTED_EDGE ( 'NONE', *, *, #22623, .F. ) ;
#6978 = VERTEX_POINT ( 'NONE', #5659 ) ;
#6980 = EDGE_CURVE ( 'NONE', #13552, #547, #5305, .T. ) ;
#6981 = DIRECTION ( 'NONE',  ( -5.551115123561405253E-17, -1.000000000000000000, -2.256980353643891447E-27 ) ) ;
#6982 = CARTESIAN_POINT ( 'NONE',  ( -50.65685424949275983, -3.200000000000108979, -8.000000000000007105 ) ) ;
#6983 = DIRECTION ( 'NONE',  ( -1.000000000000000000, 0.000000000000000000, 0.000000000000000000 ) ) ;
#6984 = FACE_OUTER_BOUND ( 'NONE', #3734, .T. ) ;
#6985 = ADVANCED_FACE ( 'NONE', ( #12466 ), #7313, .F. ) ;
#6986 = CARTESIAN_POINT ( 'NONE',  ( -8.195710046796570225, -11.98804095514285351, 6.570882465138064177 ) ) ;
#6987 = CARTESIAN_POINT ( 'NONE',  ( -90.63385214007837476, -2.700000000000084110, -7.926881151201908615 ) ) ;
#6988 = DIRECTION ( 'NONE',  ( -3.032184104443272185E-30, -1.000000000000000000, 7.395570986447005381E-32 ) ) ;
#6989 = CARTESIAN_POINT ( 'NONE',  ( 12.84999999999997300, 0.000000000000000000, -5.749999999999976907 ) ) ;
#6990 = DIRECTION ( 'NONE',  ( -2.013525853228507892E-32, -6.902532920683810383E-31, 1.000000000000000000 ) ) ;
#6991 = CARTESIAN_POINT ( 'NONE',  ( -4.000000000000058620, -2.309401076758546445, -3.433295621305388678 ) ) ;
#6992 = AXIS2_PLACEMENT_3D ( 'NONE', #19637, #22950, #12690 ) ;
#6993 = DIRECTION ( 'NONE',  ( 1.000000000000000000, -4.190823558986610327E-31, 1.733449886265890494E-32 ) ) ;
#6994 = CARTESIAN_POINT ( 'NONE',  ( -12.84999999999999964, -14.00000000000011369, -5.749999999999949374 ) ) ;
#6995 = DIRECTION ( 'NONE',  ( 0.000000000000000000, 0.000000000000000000, 1.000000000000000000 ) ) ;
#6996 = FACE_OUTER_BOUND ( 'NONE', #18198, .T. ) ;
#6997 = DIRECTION ( 'NONE',  ( -1.550910762415566494E-16, -1.000000000000000000, 8.135128085091684243E-31 ) ) ;
#6998 = VERTEX_POINT ( 'NONE', #14249 ) ;
#6999 =( NAMED_UNIT ( * ) SI_UNIT ( $, .STERADIAN. ) SOLID_ANGLE_UNIT ( ) );
#7000 = AXIS2_PLACEMENT_3D ( 'NONE', #13965, #1510, #14090 ) ;
#7002 = ORIENTED_EDGE ( 'NONE', *, *, #19177, .T. ) ;
#7001 = ORIENTED_EDGE ( 'NONE', *, *, #1615, .T. ) ;
#7003 = ORIENTED_EDGE ( 'NONE', *, *, #4398, .F. ) ;
#7005 = EDGE_LOOP ( 'NONE', ( #12511, #9190, #3946, #11205 ) ) ;
#7004 = EDGE_LOOP ( 'NONE', ( #9825, #5078, #12505, #1454 ) ) ;
#7006 =( REPRESENTATION_RELATIONSHIP ('NONE','NONE', #19450, #4297 ) REPRESENTATION_RELATIONSHIP_WITH_TRANSFORMATION ( #6120 )SHAPE_REPRESENTATION_RELATIONSHIP( ) );
#7007 = VERTEX_POINT ( 'NONE', #5432 ) ;
#7008 = ORIENTED_EDGE ( 'NONE', *, *, #9157, .T. ) ;
#7009 = FACE_OUTER_BOUND ( 'NONE', #5950, .T. ) ;
#7010 = DIRECTION ( 'NONE',  ( 3.330669073875432643E-16, 4.437342591868153746E-31, -1.000000000000000000 ) ) ;
#7011 = ORIENTED_EDGE ( 'NONE', *, *, #979, .T. ) ;
#7012 = DIRECTION ( 'NONE',  ( 3.330669073875432643E-16, 4.437342591868153746E-31, -1.000000000000000000 ) ) ;
#7013 = EDGE_CURVE ( 'NONE', #1275, #10194, #5191, .T. ) ;
#7014 = DIRECTION ( 'NONE',  ( -1.000000000000000000, 1.550910762415566494E-16, -8.566929763922626680E-48 ) ) ;
#7015 = AXIS2_PLACEMENT_3D ( 'NONE', #17866, #5402, #12321 ) ;
#7016 = DIRECTION ( 'NONE',  ( -1.000000000000000000, 4.190823558986610327E-31, -1.733449886265890494E-32 ) ) ;
#7017 = DIRECTION ( 'NONE',  ( -2.775557561562883647E-17, 3.406761633869147840E-16, -1.000000000000000000 ) ) ;
#7018 = CARTESIAN_POINT ( 'NONE',  ( -6.999999999999992006, -13.02884243125069652, 9.522727272727321335 ) ) ;
#7019 = DIRECTION ( 'NONE',  ( 1.000000000000000000, 2.699383410053119644E-30, 3.330669073875432643E-16 ) ) ;
#7020 = DIRECTION ( 'NONE',  ( 1.000000000000000000, 2.168404344970995063E-16, 0.000000000000000000 ) ) ;
#7021 = CARTESIAN_POINT ( 'NONE',  ( 83.98338480886826574, -11.64708151429766403, -6.000000000000019540 ) ) ;
#7022 = FACE_OUTER_BOUND ( 'NONE', #9919, .T. ) ;
#7023 = DIRECTION ( 'NONE',  ( -3.885780586188016830E-16, -4.437342591868156373E-31, 1.000000000000000000 ) ) ;
#7024 = VERTEX_POINT ( 'NONE', #10590 ) ;
#7025 = AXIS2_PLACEMENT_3D ( 'NONE', #9687, #756, #20395 ) ;
#7026 =( LENGTH_UNIT ( ) NAMED_UNIT ( * ) SI_UNIT ( .MILLI., .METRE. ) );
#7027 = CARTESIAN_POINT ( 'NONE',  ( 2.775557561562891351E-14, 0.5000000000000004441, -3.000000000000002665 ) ) ;
#7028 = CARTESIAN_POINT ( 'NONE',  ( 1.040834085586084257E-14, 4.500000000000003553, 0.000000000000000000 ) ) ;
#7030 = VERTEX_POINT ( 'NONE', #10709 ) ;
#7029 = ORIENTED_EDGE ( 'NONE', *, *, #21335, .F. ) ;
#7031 = AXIS2_PLACEMENT_3D ( 'NONE', #6084, #13028, #11257 ) ;
#7032 = ORIENTED_EDGE ( 'NONE', *, *, #14672, .F. ) ;
#7033 = CIRCLE ( 'NONE', #6647, 3.499999999999996003 ) ;
#7034 = ORIENTED_EDGE ( 'NONE', *, *, #16111, .F. ) ;
#7035 = VERTEX_POINT ( 'NONE', #12351 ) ;
#7036 = LINE ( 'NONE', #1836, #9921 ) ;
#7037 = DIRECTION ( 'NONE',  ( -1.000000000000000000, 1.734723475976796001E-16, 0.000000000000000000 ) ) ;
#7038 = CARTESIAN_POINT ( 'NONE',  ( 4.033901012036245959, 3.740908793663585197, -0.5205559028931702192 ) ) ;
#7039 = CARTESIAN_POINT ( 'NONE',  ( 4.050536630291686535, 3.778525289263165998, 0.5912575323401342287 ) ) ;
#7040 = VECTOR ( 'NONE', #6736, 1000.000000000000114 ) ;
#7041 = CARTESIAN_POINT ( 'NONE',  ( 30.00000000029184832, 2.999999999003851503, -5.999999999999998224 ) ) ;
#7042 = CARTESIAN_POINT ( 'NONE',  ( 0.2499999999999828748, 1.999999999999974021, -18.75000000000001066 ) ) ;
#7043 = CARTESIAN_POINT ( 'NONE',  ( 2.775557561562891351E-14, 10.99999999999998579, -0.4999999999999865663 ) ) ;
#7044 = PLANE ( 'NONE',  #17487 ) ;
#7045 = AXIS2_PLACEMENT_3D ( 'NONE', #2715, #9668, #13322 ) ;
#7046 = FACE_OUTER_BOUND ( 'NONE', #22941, .T. ) ;
#7047 = CARTESIAN_POINT ( 'NONE',  ( 37.57823792062862367, 10.91119608832010890, -10.29045043747236754 ) ) ;
#7048 = AXIS2_PLACEMENT_3D ( 'NONE', #9903, #13547, #10017 ) ;
#7049 = CARTESIAN_POINT ( 'NONE',  ( -4.330127018922234505, -2.775557561562891351E-14, -7.499999999999989342 ) ) ;
#7050 = DIRECTION ( 'NONE',  ( 1.000000000000000000, 0.000000000000000000, 1.066194817212772764E-26 ) ) ;
#7051 = CARTESIAN_POINT ( 'NONE',  ( -2.712762565638113355, 3.052587955998298241, -3.430618716626830267 ) ) ;
#7052 = EDGE_CURVE ( 'NONE', #13332, #22506, #14574, .T. ) ;
#7053 = AXIS2_PLACEMENT_3D ( 'NONE', #15843, #16190, #17738 ) ;
#7054 = CARTESIAN_POINT ( 'NONE',  ( -45.91923881554285458, 2.462384566050197954, -8.000000000000007105 ) ) ;
#7055 = DIRECTION ( 'NONE',  ( -3.885780586188016830E-16, -4.437342591868156373E-31, 1.000000000000000000 ) ) ;
#7056 = ORIENTED_EDGE ( 'NONE', *, *, #11264, .T. ) ;
#7057 = ORIENTED_EDGE ( 'NONE', *, *, #5044, .T. ) ;
#7058 = AXIS2_PLACEMENT_3D ( 'NONE', #11389, #12935, #4450 ) ;
#7059 = CIRCLE ( 'NONE', #2523, 5.500000000000046185 ) ;
#7060 = CYLINDRICAL_SURFACE ( 'NONE', #21568, 6.249999999999992006 ) ;
#7062 = EDGE_LOOP ( 'NONE', ( #8703, #7943, #8170, #7456 ) ) ;
#7061 = ORIENTED_EDGE ( 'NONE', *, *, #1321, .F. ) ;
#7063 = VECTOR ( 'NONE', #22344, 1000.000000000000000 ) ;
#7064 = LINE ( 'NONE', #23067, #17410 ) ;
#7065 = PLANE ( 'NONE',  #8136 ) ;
#7066 = DIRECTION ( 'NONE',  ( -2.172745813409348851E-17, 1.000000000000000000, 3.406761633869148826E-16 ) ) ;
#7067 =( NAMED_UNIT ( * ) PLANE_ANGLE_UNIT ( ) SI_UNIT ( $, .RADIAN. ) );
#7068 = AXIS2_PLACEMENT_3D ( 'NONE', #18152, #9210, #16021 ) ;
#7069 = ORIENTED_EDGE ( 'NONE', *, *, #16810, .F. ) ;
#7070 = CARTESIAN_POINT ( 'NONE',  ( 4.330127018922095949, 4.689110867544643568, -7.500000000000003553 ) ) ;
#7071 = DIRECTION ( 'NONE',  ( 3.885780586188016830E-16, 4.437342591868156373E-31, -1.000000000000000000 ) ) ;
#7072 = CYLINDRICAL_SURFACE ( 'NONE', #15428, 0.5000000000000025535 ) ;
#7073 = PRODUCT ( 'Half Handle', 'Half Handle', '', ( #21883 ) ) ;
#7074 = AXIS2_PLACEMENT_3D ( 'NONE', #2868, #15088, #4513 ) ;
#7075 = CARTESIAN_POINT ( 'NONE',  ( 1.317756351988315533, -3.857995168970278499, -0.04852650426606291284 ) ) ;
#7076 = EDGE_CURVE ( 'NONE', #3180, #16622, #12711, .T. ) ;
#7077 = FACE_OUTER_BOUND ( 'NONE', #2675, .T. ) ;
#7078 = FACE_OUTER_BOUND ( 'NONE', #15224, .T. ) ;
#7079 = AXIS2_PLACEMENT_3D ( 'NONE', #4886, #19618, #16075 ) ;
#7080 = CARTESIAN_POINT ( 'NONE',  ( -43.46238456605044576, 4.919238815542535725, 7.500000000000034639 ) ) ;
#7081 = CARTESIAN_POINT ( 'NONE',  ( 37.52451905283851374, 10.90849364905388974, -2.816987298107761273 ) ) ;
#7082 =( NAMED_UNIT ( * ) PLANE_ANGLE_UNIT ( ) SI_UNIT ( $, .RADIAN. ) );
#7083 = CIRCLE ( 'NONE', #21359, 0.4999999999999998335 ) ;
#7084 = EDGE_CURVE ( 'NONE', #2832, #4603, #11054, .T. ) ;
#7085 = CARTESIAN_POINT ( 'NONE',  ( 0.000000000000000000, 0.000000000000000000, 3.499999999999999556 ) ) ;
#7086 = CARTESIAN_POINT ( 'NONE',  ( 3.973110223767139626, 2.264800795684280898E-11, 3.565797985667429781 ) ) ;
#7087 = CIRCLE ( 'NONE', #18335, 0.4999999999999990563 ) ;
#7088 = EDGE_LOOP ( 'NONE', ( #18124, #22235, #5463, #12748 ) ) ;
#7089 = ADVANCED_FACE ( 'NONE', ( #23199 ), #14354, .F. ) ;
#7090 = APPLICATION_PROTOCOL_DEFINITION ( 'draft international standard', 'automotive_design', 1998, #12026 ) ;
#7091 = VECTOR ( 'NONE', #18834, 1000.000000000000000 ) ;
#7092 = EDGE_CURVE ( 'NONE', #20537, #4165, #2565, .T. ) ;
#7094 = ORIENTED_EDGE ( 'NONE', *, *, #13394, .F. ) ;
#7093 = ORIENTED_EDGE ( 'NONE', *, *, #14288, .F. ) ;
#7095 = EDGE_CURVE ( 'NONE', #9218, #6497, #18701, .T. ) ;
#7096 = VERTEX_POINT ( 'NONE', #8954 ) ;
#7098 = EDGE_LOOP ( 'NONE', ( #19108, #19342, #4135, #16977 ) ) ;
#7097 = VERTEX_POINT ( 'NONE', #7417 ) ;
#7099 = MECHANICAL_DESIGN_GEOMETRIC_PRESENTATION_REPRESENTATION (  '', ( #2189 ), #20993 ) ;
#7100 = FACE_OUTER_BOUND ( 'NONE', #12473, .T. ) ;
#7101 = DIRECTION ( 'NONE',  ( 0.000000000000000000, 0.000000000000000000, 1.000000000000000000 ) ) ;
#7102 = DIRECTION ( 'NONE',  ( -1.000000000000000000, 4.615739097524201565E-16, 0.000000000000000000 ) ) ;
#7103 = ORIENTED_EDGE ( 'NONE', *, *, #653, .T. ) ;
#7104 = DIRECTION ( 'NONE',  ( 1.454462294001240516E-30, 1.000000000000000000, 0.000000000000000000 ) ) ;
#7105 = CARTESIAN_POINT ( 'NONE',  ( -50.65685424949263904, -7.200000000000071232, -7.500000000000034639 ) ) ;
#7106 = CARTESIAN_POINT ( 'NONE',  ( 3.805574971170883281, -0.7499999999999388267, -3.000000000000007994 ) ) ;
#7108 = EDGE_CURVE ( 'NONE', #22298, #13467, #214, .T. ) ;
#7107 = DIRECTION ( 'NONE',  ( 5.551115123125677932E-17, 0.000000000000000000, -1.000000000000000000 ) ) ;
#7109 = EDGE_CURVE ( 'NONE', #5493, #9975, #1540, .T. ) ;
#7110 = DIRECTION ( 'NONE',  ( -1.000000000000000000, 1.700709290173333260E-16, 0.000000000000000000 ) ) ;
#7111 = DIRECTION ( 'NONE',  ( -0.8122328620674192923, 0.000000000000000000, -0.5833333333333257098 ) ) ;
#7112 = DIRECTION ( 'NONE',  ( 5.551115123561405253E-17, 1.000000000000000000, 2.256980353643891447E-27 ) ) ;
#7113 = DIRECTION ( 'NONE',  ( -1.000000000000000000, -2.699383410053119644E-30, -3.330669073875432643E-16 ) ) ;
#7114 = CARTESIAN_POINT ( 'NONE',  ( 12.84999999999997300, -12.50000000000002842, 5.750000000000088818 ) ) ;
#7115 = CARTESIAN_POINT ( 'NONE',  ( 86.02937988905580369, -11.02760560296348125, -6.499999999999943157 ) ) ;
#7116 = CARTESIAN_POINT ( 'NONE',  ( -4.211405944401508172, -2.460460786169425429, -3.751298493805527823 ) ) ;
#7117 = ADVANCED_FACE ( 'NONE', ( #6966 ), #1893, .F. ) ;
#7118 = CARTESIAN_POINT ( 'NONE',  ( 4.055492966679436151, -3.795017426214147171, 0.5629142681438522589 ) ) ;
#7119 = MECHANICAL_DESIGN_GEOMETRIC_PRESENTATION_REPRESENTATION (  '', ( #18367 ), #1835 ) ;
#7120 = ORIENTED_EDGE ( 'NONE', *, *, #2212, .T. ) ;
#7121 = ADVANCED_FACE ( 'NONE', ( #9639 ), #7447, .T. ) ;
#7123 = VERTEX_POINT ( 'NONE', #2344 ) ;
#7122 = ORIENTED_EDGE ( 'NONE', *, *, #22740, .T. ) ;
#7124 = EDGE_CURVE ( 'NONE', #15019, #1880, #16792, .T. ) ;
#7125 = VERTEX_POINT ( 'NONE', #9527 ) ;
#7126 = AXIS2_PLACEMENT_3D ( 'NONE', #14308, #10426, #23017 ) ;
#7128 = ORIENTED_EDGE ( 'NONE', *, *, #4345, .F. ) ;
#7127 = VERTEX_POINT ( 'NONE', #16685 ) ;
#7129 = AXIS2_PLACEMENT_3D ( 'NONE', #5364, #12407, #10419 ) ;
#7130 = VERTEX_POINT ( 'NONE', #20587 ) ;
#7131 = ORIENTED_EDGE ( 'NONE', *, *, #9989, .F. ) ;
#7132 = VERTEX_POINT ( 'NONE', #22116 ) ;
#7133 = CARTESIAN_POINT ( 'NONE',  ( -0.5000000000000420775, 1.999999999999932498, -8.000000000000035527 ) ) ;
#7134 = DIRECTION ( 'NONE',  ( -1.000000000000000000, -2.699383410053119644E-30, -3.330669073875432643E-16 ) ) ;
#7135 = CARTESIAN_POINT ( 'NONE',  ( -7.523653856849478849, -12.92037830543528010, 8.801128846369513425 ) ) ;
#7136 = STYLED_ITEM ( 'NONE', ( #5461 ), #1324 ) ;
#7137 = FACE_OUTER_BOUND ( 'NONE', #19316, .T. ) ;
#7138 = CARTESIAN_POINT ( 'NONE',  ( 110.9706201109471522, -9.453020409440265226, 6.500000000000095923 ) ) ;
#7139 = CARTESIAN_POINT ( 'NONE',  ( 7.499999999999992895, -5.999999999999981348, 6.250000000000005329 ) ) ;
#7140 = CARTESIAN_POINT ( 'NONE',  ( -1.274258131565020324, -3.883108878240975947, -3.220599429844259731 ) ) ;
#7141 = CARTESIAN_POINT ( 'NONE',  ( -91.14322581977724269, -1.179611963664228824E-13, 6.823838874241872077 ) ) ;
#7142 = SURFACE_SIDE_STYLE ('',( #8771 ) ) ;
#7143 = DIRECTION ( 'NONE',  ( 0.000000000000000000, 0.000000000000000000, 1.000000000000000000 ) ) ;
#7144 = DIRECTION ( 'NONE',  ( -0.7071067811865233699, 0.7071067811865715536, 0.000000000000000000 ) ) ;
#7145 = EDGE_CURVE ( 'NONE', #10170, #3062, #20980, .T. ) ;
#7146 = DIRECTION ( 'NONE',  ( 0.000000000000000000, -6.162975822039153854E-31, -1.000000000000000000 ) ) ;
#7147 = ORIENTED_EDGE ( 'NONE', *, *, #11533, .T. ) ;
#7148 = FACE_OUTER_BOUND ( 'NONE', #21148, .T. ) ;
#7149 = VECTOR ( 'NONE', #5994, 1000.000000000000000 ) ;
#7151 = ORIENTED_EDGE ( 'NONE', *, *, #8666, .T. ) ;
#7150 = ORIENTED_EDGE ( 'NONE', *, *, #10075, .T. ) ;
#7152 = EDGE_CURVE ( 'NONE', #22156, #8438, #1047, .T. ) ;
#7153 =( GEOMETRIC_REPRESENTATION_CONTEXT ( 3 ) GLOBAL_UNCERTAINTY_ASSIGNED_CONTEXT ( ( #16623 ) ) GLOBAL_UNIT_ASSIGNED_CONTEXT ( ( #16715, #22143, #20621 ) ) REPRESENTATION_CONTEXT ( 'NONE', 'WORKASPACE' ) );
#7154 = EDGE_LOOP ( 'NONE', ( #8420, #21242, #977, #60 ) ) ;
#7155 = LINE ( 'NONE', #17608, #156 ) ;
#7156 = CARTESIAN_POINT ( 'NONE',  ( 0.000000000000000000, 1.749999999999973799, 4.749999999999997335 ) ) ;
#7157 = CARTESIAN_POINT ( 'NONE',  ( 4.086376042167601419, 1.979461949354208938, -3.571471332069177773 ) ) ;
#7158 = DIRECTION ( 'NONE',  ( 0.7071067811865491270, 0.7071067811865461294, 1.565905175853767167E-16 ) ) ;
#7159 = DIRECTION ( 'NONE',  ( 0.000000000000000000, 6.802837160693368935E-15, 1.000000000000000000 ) ) ;
#7160 = CYLINDRICAL_SURFACE ( 'NONE', #22859, 2.000000000000015543 ) ;
#7161 = VECTOR ( 'NONE', #7699, 1000.000000000000000 ) ;
#7162 = CARTESIAN_POINT ( 'NONE',  ( 7.500000000000007105, -8.000000000000003553, 12.24999999999999645 ) ) ;
#7163 = DIRECTION ( 'NONE',  ( 1.039244538888917269E-16, -0.2588190451025179084, 0.9659258262890690894 ) ) ;
#7164 = CARTESIAN_POINT ( 'NONE',  ( -6.999999999999978684, 2.428612866367529932E-14, 11.74999999999996803 ) ) ;
#7165 = FACE_OUTER_BOUND ( 'NONE', #17634, .T. ) ;
#7166 = LINE ( 'NONE', #14449, #12900 ) ;
#7167 = DIRECTION ( 'NONE',  ( 1.000000000000000000, 1.479114197289388027E-30, -2.013525853228518840E-32 ) ) ;
#7168 = EDGE_CURVE ( 'NONE', #22149, #10662, #17576, .T. ) ;
#7169 = FILL_AREA_STYLE ('',( #17739 ) ) ;
#7170 = DIRECTION ( 'NONE',  ( 1.000000000000000000, 6.224605580259554159E-31, -2.887593071917436153E-31 ) ) ;
#7171 = CARTESIAN_POINT ( 'NONE',  ( -10.49999999999998224, -13.50000000000003020, 6.250000000000033751 ) ) ;
#7172 = ORIENTED_EDGE ( 'NONE', *, *, #12685, .T. ) ;
#7173 = EDGE_CURVE ( 'NONE', #21697, #4944, #20476, .T. ) ;
#7174 = ORIENTED_EDGE ( 'NONE', *, *, #22283, .T. ) ;
#7175 = DIRECTION ( 'NONE',  ( 1.000000000000000000, -4.440892098500651800E-16, 0.000000000000000000 ) ) ;
#7176 = VERTEX_POINT ( 'NONE', #13404 ) ;
#7177 = DIRECTION ( 'NONE',  ( 0.000000000000000000, -7.888609052210128564E-31, 1.000000000000000000 ) ) ;
#7178 = DIRECTION ( 'NONE',  ( -1.000000000000000000, 1.550910762415526064E-16, 0.000000000000000000 ) ) ;
#7179 = CARTESIAN_POINT ( 'NONE',  ( 6.999999999999977796, -11.18103031733298458, 8.693499985977936717 ) ) ;
#7180 = EDGE_CURVE ( 'NONE', #7803, #6727, #16562, .T. ) ;
#7181 = DIRECTION ( 'NONE',  ( 7.395570986446975166E-31, 3.382522293539642681E-32, 1.000000000000000000 ) ) ;
#7182 = ORIENTED_EDGE ( 'NONE', *, *, #16611, .F. ) ;
#7183 = CARTESIAN_POINT ( 'NONE',  ( -5.051814855409253902, 4.882486540518882201, 6.249999999999994671 ) ) ;
#7184 = CARTESIAN_POINT ( 'NONE',  ( -2.742413778650615086, -1.325747111984059590, -4.749999999999997335 ) ) ;
#7185 = CARTESIAN_POINT ( 'NONE',  ( -1.848892746611746769E-30, 3.061616997868387085E-16, -2.500000000000003997 ) ) ;
#7186 = DIRECTION ( 'NONE',  ( 2.775557561562891043E-17, -3.108639542312977099E-16, 1.000000000000000000 ) ) ;
#7187 = DIRECTION ( 'NONE',  ( -0.9878135252003119593, -2.699958717473711339E-16, 0.1556420233463085001 ) ) ;
#7188 = FACE_OUTER_BOUND ( 'NONE', #2756, .T. ) ;
#7189 = VECTOR ( 'NONE', #8010, 1000.000000000000000 ) ;
#7190 = CARTESIAN_POINT ( 'NONE',  ( 5.599999999999994316, 2.020725942163688504, -3.500000000000005773 ) ) ;
#7191 = FACE_OUTER_BOUND ( 'NONE', #11924, .T. ) ;
#7192 = DIRECTION ( 'NONE',  ( 0.9961946980917456562, -4.491439815345159091E-16, 0.08715574274765708340 ) ) ;
#7193 =( NAMED_UNIT ( * ) SI_UNIT ( $, .STERADIAN. ) SOLID_ANGLE_UNIT ( ) );
#7194 = EDGE_LOOP ( 'NONE', ( #16113, #11213, #15917, #7458 ) ) ;
#7195 = APPLICATION_PROTOCOL_DEFINITION ( 'draft international standard', 'automotive_design', 1998, #19880 ) ;
#7197 = VERTEX_POINT ( 'NONE', #471 ) ;
#7196 = ORIENTED_EDGE ( 'NONE', *, *, #19460, .T. ) ;
#7198 = ORIENTED_EDGE ( 'NONE', *, *, #22611, .F. ) ;
#7199 = ADVANCED_FACE ( 'NONE', ( #7645, #14819, #22000 ), #5887, .F. ) ;
#7201 = EDGE_LOOP ( 'NONE', ( #22148, #6572, #171, #12864 ) ) ;
#7200 = ORIENTED_EDGE ( 'NONE', *, *, #336, .T. ) ;
#7202 = AXIS2_PLACEMENT_3D ( 'NONE', #11619, #17025, #11500 ) ;
#7203 = AXIS2_PLACEMENT_3D ( 'NONE', #733, #2600, #21910 ) ;
#7204 = CARTESIAN_POINT ( 'NONE',  ( -3.499999999708153453, 38.99999999900385461, -26.00000000000000000 ) ) ;
#7205 = CARTESIAN_POINT ( 'NONE',  ( 0.000000000000000000, 1.749999999999973799, 4.749999999999997335 ) ) ;
#7206 = EDGE_CURVE ( 'NONE', #21696, #9536, #13975, .T. ) ;
#7207 = DIRECTION ( 'NONE',  ( 1.000000000000000000, 0.000000000000000000, 0.000000000000000000 ) ) ;
#7208 = PLANE ( 'NONE',  #15237 ) ;
#7209 = CARTESIAN_POINT ( 'NONE',  ( 0.000000000000000000, 0.000000000000000000, 0.000000000000000000 ) ) ;
#7210 = CARTESIAN_POINT ( 'NONE',  ( 31.55000000029185259, 16.99999999900385461, -19.49999999999998934 ) ) ;
#7211 = CARTESIAN_POINT ( 'NONE',  ( 36.00000000029184832, 16.99999999900385461, -29.00000000000000355 ) ) ;
#7212 = EDGE_CURVE ( 'NONE', #9707, #17275, #22815, .T. ) ;
#7213 = DIRECTION ( 'NONE',  ( 0.7071067811865464625, 0.7071067811865486830, 2.121016688166348642E-16 ) ) ;
#7214 = CARTESIAN_POINT ( 'NONE',  ( 42.50000000000017764, 0.5000000000000143219, 2.500000000000071498 ) ) ;
#7215 = FACE_OUTER_BOUND ( 'NONE', #11482, .T. ) ;
#7216 = EDGE_CURVE ( 'NONE', #22937, #20537, #18815, .T. ) ;
#7217 = DIRECTION ( 'NONE',  ( -0.000000000000000000, 1.000000000000000000, -0.000000000000000000 ) ) ;
#7218 = CARTESIAN_POINT ( 'NONE',  ( 114.8016533820239573, -4.500000000000059508, -6.499999999999964473 ) ) ;
#7219 = AXIS2_PLACEMENT_3D ( 'NONE', #19015, #17232, #15809 ) ;
#7220 = AXIS2_PLACEMENT_3D ( 'NONE', #22975, #14143, #11158 ) ;
#7221 = CARTESIAN_POINT ( 'NONE',  ( -6.962001439796694058, 35.99999999900384751, -18.52402997057235723 ) ) ;
#7222 = FACE_OUTER_BOUND ( 'NONE', #19805, .T. ) ;
#7223 = VERTEX_POINT ( 'NONE', #6464 ) ;
#7225 = ORIENTED_EDGE ( 'NONE', *, *, #9053, .F. ) ;
#7224 = EDGE_LOOP ( 'NONE', ( #9916, #4145, #20857, #11267 ) ) ;
#7226 = EDGE_LOOP ( 'NONE', ( #828, #7029, #3454, #13204 ) ) ;
#7227 = ADVANCED_FACE ( 'NONE', ( #10110 ), #21052, .T. ) ;
#7228 = ADVANCED_FACE ( 'NONE', ( #9997 ), #3049, .F. ) ;
#7230 = VERTEX_POINT ( 'NONE', #17150 ) ;
#7229 = VERTEX_POINT ( 'NONE', #8575 ) ;
#7231 = AXIS2_PLACEMENT_3D ( 'NONE', #18633, #4271, #21946 ) ;
#7232 = ORIENTED_EDGE ( 'NONE', *, *, #1371, .F. ) ;
#7233 = ORIENTED_EDGE ( 'NONE', *, *, #6824, .F. ) ;
#7234 = EDGE_CURVE ( 'NONE', #20801, #10484, #20118, .T. ) ;
#7235 = ORIENTED_EDGE ( 'NONE', *, *, #174, .T. ) ;
#7236 = FACE_OUTER_BOUND ( 'NONE', #20967, .T. ) ;
#7237 = CIRCLE ( 'NONE', #1942, 2.500000000000003997 ) ;
#7238 = VECTOR ( 'NONE', #9720, 1000.000000000000000 ) ;
#7239 = CARTESIAN_POINT ( 'NONE',  ( -8.954763739086866181, -13.50000000000003553, 6.678571428571478563 ) ) ;
#7240 = AXIS2_PLACEMENT_3D ( 'NONE', #7041, #12191, #3276 ) ;
#7241 = DIRECTION ( 'NONE',  ( 0.000000000000000000, 0.000000000000000000, -1.000000000000000000 ) ) ;
#7242 = EDGE_CURVE ( 'NONE', #13332, #6496, #1064, .T. ) ;
#7243 = ADVANCED_BREP_SHAPE_REPRESENTATION ( '', ( #13034, #22115 ), #14985 ) ;
#7244 = CARTESIAN_POINT ( 'NONE',  ( -3.861362476283353384, -2.629030857716048608, -3.671615880910375385 ) ) ;
#7245 = DIRECTION ( 'NONE',  ( 1.000000000000000000, 2.168404344971017743E-16, -1.780660105995169760E-30 ) ) ;
#7246 = EDGE_CURVE ( 'NONE', #15368, #12647, #17034, .T. ) ;
#7247 = CARTESIAN_POINT ( 'NONE',  ( -1.287237434361804045, -3.875615274277503186, -3.430618716626840925 ) ) ;
#7248 = CARTESIAN_POINT ( 'NONE',  ( -67.28510754798018922, 0.5000000000000143219, 12.22107821754958579 ) ) ;
#7249 = CARTESIAN_POINT ( 'NONE',  ( 37.43301270189233776, 10.75000000000000000, -9.999999999999994671 ) ) ;
#7250 = CARTESIAN_POINT ( 'NONE',  ( 26.45000000029184051, 16.99999999900385461, -25.50000000000000355 ) ) ;
#7251 = CARTESIAN_POINT ( 'NONE',  ( 4.175813232069149450, 4.122719923832687705, 1.040834085586084257E-14 ) ) ;
#7252 = ORIENTED_EDGE ( 'NONE', *, *, #9695, .T. ) ;
#7253 = PLANE ( 'NONE',  #7126 ) ;
#7254 = CIRCLE ( 'NONE', #20394, 7.499999999999998224 ) ;
#7256 = VERTEX_POINT ( 'NONE', #8111 ) ;
#7255 = VERTEX_POINT ( 'NONE', #4808 ) ;
#7257 = VECTOR ( 'NONE', #8423, 1000.000000000000000 ) ;
#7258 = VECTOR ( 'NONE', #18894, 1000.000000000000000 ) ;
#7259 = EDGE_CURVE ( 'NONE', #2262, #1131, #10828, .T. ) ;
#7260 = VECTOR ( 'NONE', #20046, 1000.000000000000000 ) ;
#7261 = EDGE_CURVE ( 'NONE', #13207, #1275, #17596, .T. ) ;
#7262 = ORIENTED_EDGE ( 'NONE', *, *, #6232, .T. ) ;
#7263 = ORIENTED_EDGE ( 'NONE', *, *, #17401, .T. ) ;
#7264 = DIRECTION ( 'NONE',  ( 1.000000000000000000, 4.440892098500626162E-16, 5.551115123125782702E-16 ) ) ;
#7265 = DIRECTION ( 'NONE',  ( 1.000000000000000000, -1.276756478318923119E-15, 1.387778780781436998E-15 ) ) ;
#7266 = EDGE_CURVE ( 'NONE', #3149, #16593, #15340, .T. ) ;
#7267 = DIRECTION ( 'NONE',  ( 1.000000000000000000, -4.615739097524200579E-16, -1.134196829589820086E-15 ) ) ;
#7268 = CARTESIAN_POINT ( 'NONE',  ( 4.050823680195226650, -2.400527758044912474, -2.978030508226150452 ) ) ;
#7269 = CIRCLE ( 'NONE', #20429, 10.00000000000006395 ) ;
#7270 = EDGE_CURVE ( 'NONE', #21059, #9302, #2820, .T. ) ;
#7271 = CARTESIAN_POINT ( 'NONE',  ( 12.84999999999997300, -14.00000000000007105, 5.551115123125782702E-14 ) ) ;
#7272 = AXIS2_PLACEMENT_3D ( 'NONE', #21336, #12370, #19553 ) ;
#7273 = CARTESIAN_POINT ( 'NONE',  ( -89.70000000000064233, 0.5000000000000490719, -2.000000000000001776 ) ) ;
#7274 = FACE_OUTER_BOUND ( 'NONE', #572, .T. ) ;
#7275 = AXIS2_PLACEMENT_3D ( 'NONE', #14235, #3305, #17881 ) ;
#7276 = CIRCLE ( 'NONE', #4637, 6.000000000000037303 ) ;
#7277 = DIRECTION ( 'NONE',  ( 3.885780586188016830E-16, 4.437342591868156373E-31, -1.000000000000000000 ) ) ;
#7278 = CIRCLE ( 'NONE', #15129, 0.2500000000000000000 ) ;
#7279 = COLOUR_RGB ( '', 0.66274510, 0.83137255, 0.94901961) ;
#7280 = CARTESIAN_POINT ( 'NONE',  ( -7.000000000000020428, -2.818969682667033183, 8.693499985977942046 ) ) ;
#7281 = CARTESIAN_POINT ( 'NONE',  ( 37.04362427881607545, 10.78777973366380216, -10.45482484129298051 ) ) ;
#7282 = DIRECTION ( 'NONE',  ( -0.9706398123736329486, 1.505375731439247187E-16, -0.2405376366294442458 ) ) ;
#7283 = DIRECTION ( 'NONE',  ( 2.168404344971017743E-16, 1.000000000000000000, -6.982962677686261977E-15 ) ) ;
#7284 = CARTESIAN_POINT ( 'NONE',  ( -3.522875095020107317, 2.820352903224537577, -3.598441714920560752 ) ) ;
#7285 = DIRECTION ( 'NONE',  ( -1.000000000000000000, 1.550910762415566494E-16, -8.566929763922626680E-48 ) ) ;
#7286 = FACE_OUTER_BOUND ( 'NONE', #12453, .T. ) ;
#7287 = ORIENTED_EDGE ( 'NONE', *, *, #9516, .T. ) ;
#7288 = CONICAL_SURFACE ( 'NONE', #10259, 3.500000000000004441, 1.047197551196600296 ) ;
#7289 = CIRCLE ( 'NONE', #15527, 0.4999999999999987232 ) ;
#7290 = ORIENTED_EDGE ( 'NONE', *, *, #18015, .F. ) ;
#7291 = AXIS2_PLACEMENT_3D ( 'NONE', #11161, #16551, #5876 ) ;
#7292 = CIRCLE ( 'NONE', #2391, 5.200000000000001066 ) ;
#7293 = DIRECTION ( 'NONE',  ( 1.000000000000000000, 3.254448077276381206E-32, 1.066788928082016908E-26 ) ) ;
#7294 = EDGE_CURVE ( 'NONE', #19001, #3406, #6722, .T. ) ;
#7295 = ORIENTED_EDGE ( 'NONE', *, *, #15709, .F. ) ;
#7296 = CARTESIAN_POINT ( 'NONE',  ( -3.191783008269798660, -1.561572887838416079, -3.971669662941494927 ) ) ;
#7297 = CARTESIAN_POINT ( 'NONE',  ( 2.499999999999992006, 4.250000000000003553, -3.469446951953614189E-14 ) ) ;
#7298 = CARTESIAN_POINT ( 'NONE',  ( 77.42435809754135789, -3.999999999999809042, 6.500000000000137668 ) ) ;
#7299 = DIRECTION ( 'NONE',  ( 1.000000000000000000, 1.144237745222090235E-17, -1.939787525279694125E-32 ) ) ;
#7300 = ORIENTED_EDGE ( 'NONE', *, *, #10778, .T. ) ;
#7301 = DIRECTION ( 'NONE',  ( 1.000000000000000000, 0.000000000000000000, 0.000000000000000000 ) ) ;
#7302 = DIRECTION ( 'NONE',  ( -1.000000000000000000, 6.640738306473671271E-15, 4.480856046118915636E-31 ) ) ;
#7303 = DIRECTION ( 'NONE',  ( 0.000000000000000000, 0.000000000000000000, 1.000000000000000000 ) ) ;
#7304 = EDGE_CURVE ( 'NONE', #10857, #8955, #13473, .T. ) ;
#7305 = CARTESIAN_POINT ( 'NONE',  ( -5.551115123125782702E-14, 4.618802153517065356, -0.5000000000000004441 ) ) ;
#7306 = CARTESIAN_POINT ( 'NONE',  ( -55.25320565519140104, -2.700000000000049472, 10.00000000000007816 ) ) ;
#7307 = FACE_OUTER_BOUND ( 'NONE', #18534, .T. ) ;
#7308 = CIRCLE ( 'NONE', #15909, 7.500000000000001776 ) ;
#7309 = CARTESIAN_POINT ( 'NONE',  ( -4.000000000000003553, 2.309401076758494487, -0.3572655899081629283 ) ) ;
#7310 = FACE_OUTER_BOUND ( 'NONE', #13093, .T. ) ;
#7311 = AXIS2_PLACEMENT_3D ( 'NONE', #12989, #20164, #21819 ) ;
#7312 = CARTESIAN_POINT ( 'NONE',  ( -3.534277608972057561, 1.672424706883767875, 3.378451613207333448 ) ) ;
#7313 = CYLINDRICAL_SURFACE ( 'NONE', #9713, 2.550000000000002043 ) ;
#7314 = ORIENTED_EDGE ( 'NONE', *, *, #3301, .T. ) ;
#7315 = APPLICATION_PROTOCOL_DEFINITION ( 'draft international standard', 'automotive_design', 1998, #17783 ) ;
#7317 = ORIENTED_EDGE ( 'NONE', *, *, #12256, .F. ) ;
#7316 = ORIENTED_EDGE ( 'NONE', *, *, #19074, .T. ) ;
#7318 = ORIENTED_EDGE ( 'NONE', *, *, #186, .T. ) ;
#7319 = AXIS2_PLACEMENT_3D ( 'NONE', #12728, #1791, #16128 ) ;
#7321 = VERTEX_POINT ( 'NONE', #20704 ) ;
#7320 = EDGE_LOOP ( 'NONE', ( #9337, #11847, #14534 ) ) ;
#7322 = AXIS2_PLACEMENT_3D ( 'NONE', #11438, #2502, #13450 ) ;
#7323 = VECTOR ( 'NONE', #21073, 1000.000000000000000 ) ;
#7324 = CARTESIAN_POINT ( 'NONE',  ( 3.472371940586146177, 2.614027278893112261, -3.320322319202220651 ) ) ;
#7325 = CARTESIAN_POINT ( 'NONE',  ( 8.414481090081473269, 1.737226928909803488E-14, 6.435353702847417701 ) ) ;
#7326 = CARTESIAN_POINT ( 'NONE',  ( 5.600000000000000533, 1.758911592640616865E-31, 5.200000000000004619 ) ) ;
#7327 = DIRECTION ( 'NONE',  ( 2.220446049250313081E-16, -1.000000000000000000, 7.025792437124636392E-31 ) ) ;
#7328 = SURFACE_STYLE_USAGE ( .BOTH. , #12244 ) ;
#7329 = CARTESIAN_POINT ( 'NONE',  ( 2.130086964121806377E-14, 10.00000000000000533, 2.500000000000000000 ) ) ;
#7330 = FACE_OUTER_BOUND ( 'NONE', #16832, .T. ) ;
#7331 = DIRECTION ( 'NONE',  ( 0.000000000000000000, 0.000000000000000000, 1.000000000000000000 ) ) ;
#7332 = DIRECTION ( 'NONE',  ( 0.000000000000000000, -6.938893903907237055E-15, -1.000000000000000000 ) ) ;
#7333 = DIRECTION ( 'NONE',  ( 0.7313537016191735685, -0.6819983600624951459, 3.923113172947598083E-16 ) ) ;
#7334 = CIRCLE ( 'NONE', #201, 0.8000000000000090372 ) ;
#7335 = AXIS2_PLACEMENT_3D ( 'NONE', #21219, #8497, #19548 ) ;
#7336 = DIRECTION ( 'NONE',  ( 1.000000000000000000, 2.699383410053119644E-30, 3.330669073875432643E-16 ) ) ;
#7337 = CARTESIAN_POINT ( 'NONE',  ( -67.28510754798023186, 3.200000000000022382, 12.22107821754961421 ) ) ;
#7338 = DIRECTION ( 'NONE',  ( 0.3420201433256626622, 1.518874552022986003E-16, -0.9396926207859105373 ) ) ;
#7339 = ORIENTED_EDGE ( 'NONE', *, *, #11419, .T. ) ;
#7340 = EDGE_CURVE ( 'NONE', #180, #5339, #19483, .T. ) ;
#7341 =( NAMED_UNIT ( * ) SI_UNIT ( $, .STERADIAN. ) SOLID_ANGLE_UNIT ( ) );
#7343 = ORIENTED_EDGE ( 'NONE', *, *, #11284, .T. ) ;
#7342 = EDGE_LOOP ( 'NONE', ( #15452, #8494, #10513, #8894, #1435, #10833 ) ) ;
#7344 = ORIENTED_EDGE ( 'NONE', *, *, #6662, .F. ) ;
#7346 = ORIENTED_EDGE ( 'NONE', *, *, #14053, .F. ) ;
#7345 = VERTEX_POINT ( 'NONE', #15506 ) ;
#7347 = ORIENTED_EDGE ( 'NONE', *, *, #11113, .T. ) ;
#7348 = CYLINDRICAL_SURFACE ( 'NONE', #12095, 4.000000000000023981 ) ;
#7349 = ORIENTED_EDGE ( 'NONE', *, *, #2620, .T. ) ;
#7350 = ORIENTED_EDGE ( 'NONE', *, *, #17893, .T. ) ;
#7351 = LINE ( 'NONE', #68, #5043 ) ;
#7352 = AXIS2_PLACEMENT_3D ( 'NONE', #6822, #13766, #21424 ) ;
#7353 = CYLINDRICAL_SURFACE ( 'NONE', #755, 10.00000000000006395 ) ;
#7354 = CARTESIAN_POINT ( 'NONE',  ( -2.081668171172168513E-14, 4.618802153517051146, 0.000000000000000000 ) ) ;
#7355 = CARTESIAN_POINT ( 'NONE',  ( 4.170895651974845464, -2.054890354522496132, -3.559174498016470345 ) ) ;
#7356 = DIRECTION ( 'NONE',  ( 1.000000000000000000, -1.424116703980815236E-16, -2.931272055834072749E-32 ) ) ;
#7357 = FACE_OUTER_BOUND ( 'NONE', #13331, .T. ) ;
#7358 = FILL_AREA_STYLE_COLOUR ( '', #13399 ) ;
#7359 = EDGE_CURVE ( 'NONE', #20629, #20539, #16842, .T. ) ;
#7360 = CARTESIAN_POINT ( 'NONE',  ( 2.081668171172168513E-14, 10.00000000000000533, 0.000000000000000000 ) ) ;
#7361 = AXIS2_PLACEMENT_3D ( 'NONE', #9149, #19742, #2194 ) ;
#7362 = DIRECTION ( 'NONE',  ( 1.000000000000000000, 2.168404344970994323E-16, -1.780660105995169760E-30 ) ) ;
#7363 = CARTESIAN_POINT ( 'NONE',  ( 37.09721192198001916, 10.82270004028423394, -2.518381337117829410 ) ) ;
#7364 = EDGE_LOOP ( 'NONE', ( #15684, #11575, #13126, #11930 ) ) ;
#7365 = ADVANCED_FACE ( 'NONE', ( #16193 ), #13100, .T. ) ;
#7366 =( NAMED_UNIT ( * ) SI_UNIT ( $, .STERADIAN. ) SOLID_ANGLE_UNIT ( ) );
#7367 = CARTESIAN_POINT ( 'NONE',  ( 6.000000000291855429, 2.999999999003851503, -45.00000000000000000 ) ) ;
#7369 = ORIENTED_EDGE ( 'NONE', *, *, #14686, .F. ) ;
#7368 = EDGE_LOOP ( 'NONE', ( #20781, #8993, #3181, #13708, #20044 ) ) ;
#7370 = ORIENTED_EDGE ( 'NONE', *, *, #18745, .F. ) ;
#7371 = EDGE_CURVE ( 'NONE', #6724, #4343, #2198, .T. ) ;
#7372 = EDGE_LOOP ( 'NONE', ( #21559, #13622, #13620, #18767, #18201, #12948, #18388, #20658 ) ) ;
#7373 = ADVANCED_FACE ( 'NONE', ( #3631 ), #12561, .T. ) ;
#7374 = ADVANCED_FACE ( 'NONE', ( #5160 ), #18094, .F. ) ;
#7375 = ORIENTED_EDGE ( 'NONE', *, *, #20908, .T. ) ;
#7376 = VECTOR ( 'NONE', #824, 1000.000000000000000 ) ;
#7377 = CARTESIAN_POINT ( 'NONE',  ( 30.00000000029184832, -9.961476088449217059E-10, -3.449999999999999289 ) ) ;
#7378 = DIRECTION ( 'NONE',  ( 0.000000000000000000, 0.000000000000000000, 1.000000000000000000 ) ) ;
#7379 = PLANE ( 'NONE',  #18108 ) ;
#7380 = DIRECTION ( 'NONE',  ( 0.6819983600624981435, -0.7313537016191709039, 0.000000000000000000 ) ) ;
#7381 = FACE_OUTER_BOUND ( 'NONE', #18302, .T. ) ;
#7382 = ADVANCED_FACE ( 'NONE', ( #1853 ), #5607, .T. ) ;
#7383 = ADVANCED_FACE ( 'NONE', ( #12439 ), #1963, .F. ) ;
#7384 = LINE ( 'NONE', #14447, #13201 ) ;
#7385 = EDGE_CURVE ( 'NONE', #15168, #14019, #21740, .T. ) ;
#7386 = CARTESIAN_POINT ( 'NONE',  ( 27.94974746859769255, 27.94974746730969528, -15.99999999999999289 ) ) ;
#7387 = LINE ( 'NONE', #21850, #14794 ) ;
#7388 = CARTESIAN_POINT ( 'NONE',  ( 37.09721192198001916, 0.1772999597158308738, -10.48161866288212885 ) ) ;
#7389 = AXIS2_PLACEMENT_3D ( 'NONE', #22784, #6658, #22321 ) ;
#7390 = VECTOR ( 'NONE', #5715, 1000.000000000000000 ) ;
#7391 = CARTESIAN_POINT ( 'NONE',  ( -95.20000000000067075, 0.5000000000000073275, -1.999999999999974021 ) ) ;
#7392 = CARTESIAN_POINT ( 'NONE',  ( 4.175813232069149450, -4.122719923832729449, 0.000000000000000000 ) ) ;
#7393 = VERTEX_POINT ( 'NONE', #19624 ) ;
#7394 = EDGE_CURVE ( 'NONE', #10194, #6184, #2960, .T. ) ;
#7395 = EDGE_CURVE ( 'NONE', #9105, #10170, #6934, .T. ) ;
#7396 = ORIENTED_EDGE ( 'NONE', *, *, #21338, .F. ) ;
#7397 = CARTESIAN_POINT ( 'NONE',  ( -3.336453936897160411, -2.700000000000098321, -21.17547853860576978 ) ) ;
#7398 = CARTESIAN_POINT ( 'NONE',  ( 58.04599508018841192, 2.194061104857452982, 6.500000000000199840 ) ) ;
#7399 = ORIENTED_EDGE ( 'NONE', *, *, #12376, .T. ) ;
#7400 = VECTOR ( 'NONE', #4556, 1000.000000000000000 ) ;
#7401 = CARTESIAN_POINT ( 'NONE',  ( -12.84999999999999964, -1.499999999999997780, 6.250000000000033751 ) ) ;
#7402 = LINE ( 'NONE', #7742, #12248 ) ;
#7403 = LINE ( 'NONE', #349, #11841 ) ;
#7404 = VECTOR ( 'NONE', #22936, 1000.000000000000000 ) ;
#7405 = CARTESIAN_POINT ( 'NONE',  ( 0.000000000000000000, 0.000000000000000000, -5.600000000000000533 ) ) ;
#7406 = CIRCLE ( 'NONE', #5154, 6.500000000000075495 ) ;
#7407 = ORIENTED_EDGE ( 'NONE', *, *, #17149, .T. ) ;
#7408 = DIRECTION ( 'NONE',  ( 1.000000000000000000, 0.000000000000000000, 0.000000000000000000 ) ) ;
#7409 = CARTESIAN_POINT ( 'NONE',  ( -2.296348136152779329, -1.454515171370276860, -4.750000000000026645 ) ) ;
#7410 = CARTESIAN_POINT ( 'NONE',  ( -42.54314575050785407, -8.000000000000021316, 8.000000000000007105 ) ) ;
#7411 = DIRECTION ( 'NONE',  ( -0.000000000000000000, -0.000000000000000000, -1.000000000000000000 ) ) ;
#7412 = CARTESIAN_POINT ( 'NONE',  ( 8.429621201838076061, -14.00000000000004974, 6.425428529986020543 ) ) ;
#7413 = DIRECTION ( 'NONE',  ( 0.7071067811865475727, 0.7071067811865475727, 0.000000000000000000 ) ) ;
#7414 = DIRECTION ( 'NONE',  ( 1.000000000000000000, 3.254448077276381206E-32, 1.066788928082016908E-26 ) ) ;
#7415 = LINE ( 'NONE', #19994, #19464 ) ;
#7416 = SURFACE_SIDE_STYLE ('',( #18352 ) ) ;
#7417 = CARTESIAN_POINT ( 'NONE',  ( 3.999999999999989786, -2.309401076758549998, -5.242734410091827613 ) ) ;
#7418 = AXIS2_PLACEMENT_3D ( 'NONE', #2456, #13172, #18811 ) ;
#7419 = EDGE_CURVE ( 'NONE', #6879, #17750, #11218, .T. ) ;
#7420 = AXIS2_PLACEMENT_3D ( 'NONE', #224, #19513, #10455 ) ;
#7421 = SHAPE_DEFINITION_REPRESENTATION ( #17764, #9834 ) ;
#7422 = ADVANCED_FACE ( 'NONE', ( #14556 ), #17218, .T. ) ;
#7424 = ORIENTED_EDGE ( 'NONE', *, *, #11852, .T. ) ;
#7423 = ORIENTED_EDGE ( 'NONE', *, *, #12128, .F. ) ;
#7425 = ADVANCED_FACE ( 'NONE', ( #109 ), #23172, .T. ) ;
#7426 = VECTOR ( 'NONE', #19443, 1000.000000000000000 ) ;
#7428 = EDGE_LOOP ( 'NONE', ( #22265, #15582, #10143, #10120 ) ) ;
#7427 = ORIENTED_EDGE ( 'NONE', *, *, #14825, .F. ) ;
#7429 = LINE ( 'NONE', #18248, #19302 ) ;
#7430 = CIRCLE ( 'NONE', #10065, 2.250000000000001776 ) ;
#7431 = CARTESIAN_POINT ( 'NONE',  ( 37.57823792062836787, 0.08880391168000995039, -2.709549562527593825 ) ) ;
#7432 = CARTESIAN_POINT ( 'NONE',  ( 7.778057173929708412, -12.23790148979555070, 7.981635986975476271 ) ) ;
#7433 =( BOUNDED_SURFACE ( )  B_SPLINE_SURFACE ( 3, 2, ( 
 ( #6052, #16617, #2512 ),
 ( #13111, #11449, #18516 ),
 ( #13221, #20405, #2634 ),
 ( #9810, #3101, #8284 ),
 ( #13693, #4854, #15666 ),
 ( #10381, #20985, #19097 ) ),
 .UNSPECIFIED., .F., .F., .F. ) 
 B_SPLINE_SURFACE_WITH_KNOTS ( ( 4, 2, 4 ),
 ( 3, 3 ),
 ( 0.01651732063679903564, 0.01857756227444015695, 0.02063780391208127479 ),
 ( 0.000000000000000000, 1.000000000000000000 ),
 .UNSPECIFIED. ) 
 GEOMETRIC_REPRESENTATION_ITEM ( )  RATIONAL_B_SPLINE_SURFACE ( (
 ( 1.000000000000000000, 0.8047781231227471022, 1.000000000000000000),
 ( 1.000000000000000000, 0.8123782108667384483, 1.000000000000000000),
 ( 1.000000000000000000, 0.8190665102130285646, 1.000000000000000000),
 ( 1.000000000000000000, 0.8192358432847179905, 1.000000000000000000),
 ( 1.000000000000000000, 0.8126132624432910179, 1.000000000000000000),
 ( 1.000000000000000000, 0.8047712436238864120, 1.000000000000000000) ) ) 
 REPRESENTATION_ITEM ( '' )  SURFACE ( )  );
#7434 = DIRECTION ( 'NONE',  ( 0.000000000000000000, 0.000000000000000000, 1.000000000000000000 ) ) ;
#7435 = CIRCLE ( 'NONE', #21355, 0.4999999999999995559 ) ;
#7436 = DIRECTION ( 'NONE',  ( 1.000000000000000000, 4.252453317207022018E-31, -5.551115123125818447E-17 ) ) ;
#7437 = CARTESIAN_POINT ( 'NONE',  ( 119.5756419024615553, -11.00000000000006573, 6.500000000000012434 ) ) ;
#7438 = AXIS2_PLACEMENT_3D ( 'NONE', #769, #7932, #12255 ) ;
#7439 = CARTESIAN_POINT ( 'NONE',  ( 0.1422498215951156220, -0.5999999999999894307, 3.724967290803227193 ) ) ;
#7440 = CARTESIAN_POINT ( 'NONE',  ( 108.2426266706970779, -6.527605602963587828, 6.000000000000109246 ) ) ;
#7441 = CARTESIAN_POINT ( 'NONE',  ( 4.630153689607049650, 6.577590292450094690E-16, 5.371010071662835728 ) ) ;
#7442 = CARTESIAN_POINT ( 'NONE',  ( -6.938893903907228378E-14, 4.999999999999976907, -4.163336342344337027E-14 ) ) ;
#7444 = CIRCLE ( 'NONE', #2942, 0.5000000000000038858 ) ;
#7443 = APPLICATION_CONTEXT ( 'automotive_design' ) ;
#7445 = FACE_OUTER_BOUND ( 'NONE', #21060, .T. ) ;
#7446 = DIRECTION ( 'NONE',  ( -0.2405376366294442736, 3.887513393996810040E-17, 0.9706398123736330597 ) ) ;
#7447 = CONICAL_SURFACE ( 'NONE', #10449, 3.499999999999999556, 1.047197551196600074 ) ;
#7448 = CARTESIAN_POINT ( 'NONE',  ( -12.84999999999999964, -1.500000000000001332, 0.000000000000000000 ) ) ;
#7449 = FACE_OUTER_BOUND ( 'NONE', #9790, .T. ) ;
#7450 = CARTESIAN_POINT ( 'NONE',  ( 0.1217565302851134484, 3.710888496608927056, -0.5725525826504704874 ) ) ;
#7451 = EDGE_LOOP ( 'NONE', ( #4057, #10408, #21362, #19699 ) ) ;
#7452 =( NAMED_UNIT ( * ) SI_UNIT ( $, .STERADIAN. ) SOLID_ANGLE_UNIT ( ) );
#7454 = ORIENTED_EDGE ( 'NONE', *, *, #7975, .T. ) ;
#7453 = ORIENTED_EDGE ( 'NONE', *, *, #14993, .F. ) ;
#7455 = UNCERTAINTY_MEASURE_WITH_UNIT (LENGTH_MEASURE( 1.000000000000000082E-05 ), #17648, 'distance_accuracy_value', 'NONE');
#7456 = ORIENTED_EDGE ( 'NONE', *, *, #21108, .T. ) ;
#7458 = ORIENTED_EDGE ( 'NONE', *, *, #16140, .F. ) ;
#7457 = ORIENTED_EDGE ( 'NONE', *, *, #5389, .T. ) ;
#7459 = AXIS2_PLACEMENT_3D ( 'NONE', #9865, #1167, #3040 ) ;
#7460 = VERTEX_POINT ( 'NONE', #3288 ) ;
#7461 = CARTESIAN_POINT ( 'NONE',  ( 88.75737332930594903, -6.527605602963476805, 6.500000000000151879 ) ) ;
#7462 = ORIENTED_EDGE ( 'NONE', *, *, #17174, .T. ) ;
#7463 = VERTEX_POINT ( 'NONE', #1 ) ;
#7464 = DIRECTION ( 'NONE',  ( -0.4472135954999518215, 0.7745966692414842925, 0.4472135954999624796 ) ) ;
#7465 = CIRCLE ( 'NONE', #10461, 4.750000000000000000 ) ;
#7466 = AXIS2_PLACEMENT_3D ( 'NONE', #3472, #19822, #19354 ) ;
#7467 = DIRECTION ( 'NONE',  ( 0.000000000000000000, 0.000000000000000000, 1.000000000000000000 ) ) ;
#7468 = CARTESIAN_POINT ( 'NONE',  ( 0.000000000000000000, 0.000000000000000000, 3.469446951953614189E-15 ) ) ;
#7469 = LINE ( 'NONE', #15922, #9864 ) ;
#7470 = ADVANCED_FACE ( 'NONE', ( #23051 ), #1739, .T. ) ;
#7471 = CYLINDRICAL_SURFACE ( 'NONE', #13257, 0.5000000000000037748 ) ;
#7472 = DIRECTION ( 'NONE',  ( 3.241725282392603095E-30, 1.000000000000000000, -2.218671295934100958E-31 ) ) ;
#7473 = DIRECTION ( 'NONE',  ( 2.013525853228507892E-32, 6.902532920683810383E-31, -1.000000000000000000 ) ) ;
#7474 = CARTESIAN_POINT ( 'NONE',  ( 5.600000000000000533, 2.020725942163612121, 3.499999999999957812 ) ) ;
#7475 =( GEOMETRIC_REPRESENTATION_CONTEXT ( 3 ) GLOBAL_UNCERTAINTY_ASSIGNED_CONTEXT ( ( #13787 ) ) GLOBAL_UNIT_ASSIGNED_CONTEXT ( ( #7026, #8896, #21494 ) ) REPRESENTATION_CONTEXT ( 'NONE', 'WORKASPACE' ) );
#7476 = DIRECTION ( 'NONE',  ( -1.000000000000000000, 1.276756478318922725E-15, -1.333893503340766402E-15 ) ) ;
#7477 = ORIENTED_EDGE ( 'NONE', *, *, #21338, .T. ) ;
#7478 = VECTOR ( 'NONE', #9264, 1000.000000000000000 ) ;
#7479 = CARTESIAN_POINT ( 'NONE',  ( -65.00000000000052580, 2.700000000000063238, 3.000000000000002665 ) ) ;
#7480 = B_SPLINE_CURVE_WITH_KNOTS ( 'NONE', 3,
 ( #7972, #18672, #6215, #20687, #15371, #13384 ),
 .UNSPECIFIED., .F., .F.,
 ( 4, 2, 4 ),
 ( 0.006456566858647396628, 0.007625406818786667311, 0.008794246778925937993 ),
 .UNSPECIFIED. ) ;
#7482 = ORIENTED_EDGE ( 'NONE', *, *, #8881, .F. ) ;
#7481 = ORIENTED_EDGE ( 'NONE', *, *, #5616, .T. ) ;
#7483 = VERTEX_POINT ( 'NONE', #1629 ) ;
#7484 = ORIENTED_EDGE ( 'NONE', *, *, #12530, .F. ) ;
#7485 = VERTEX_POINT ( 'NONE', #7054 ) ;
#7486 = ORIENTED_EDGE ( 'NONE', *, *, #2803, .F. ) ;
#7487 = ADVANCED_FACE ( 'NONE', ( #21523 ), #23262, .T. ) ;
#7488 = FACE_OUTER_BOUND ( 'NONE', #714, .T. ) ;
#7489 = LINE ( 'NONE', #14658, #7613 ) ;
#7490 = CARTESIAN_POINT ( 'NONE',  ( 4.175813232069142344, 4.122719923832743660, 0.000000000000000000 ) ) ;
#7491 = EDGE_CURVE ( 'NONE', #9423, #18520, #9454, .T. ) ;
#7492 = AXIS2_PLACEMENT_3D ( 'NONE', #14267, #19681, #9200 ) ;
#7493 = DIRECTION ( 'NONE',  ( -2.013525853228507892E-32, -6.902532920683810383E-31, 1.000000000000000000 ) ) ;
#7494 = DIRECTION ( 'NONE',  ( -0.000000000000000000, -0.000000000000000000, 1.000000000000000000 ) ) ;
#7495 = CARTESIAN_POINT ( 'NONE',  ( -50.65685424949267457, 7.200000000000018829, -7.500000000000034639 ) ) ;
#7496 = CYLINDRICAL_SURFACE ( 'NONE', #9258, 6.000000000000047073 ) ;
#7497 = CARTESIAN_POINT ( 'NONE',  ( -7.499999999999988454, -12.78258024831861661, 9.022398393215850021 ) ) ;
#7498 = LINE ( 'NONE', #18319, #2160 ) ;
#7499 = ADVANCED_FACE ( 'NONE', ( #11480 ), #12791, .T. ) ;
#7501 = EDGE_CURVE ( 'NONE', #1178, #13386, #17994, .T. ) ;
#7500 = CIRCLE ( 'NONE', #6381, 2.500000000000003997 ) ;
#7502 = LINE ( 'NONE', #22198, #16279 ) ;
#7503 = FACE_OUTER_BOUND ( 'NONE', #4364, .T. ) ;
#7505 = ADVANCED_FACE ( 'NONE', ( #16536 ), #684, .T. ) ;
#7504 = DIRECTION ( 'NONE',  ( -1.000000000000000000, 2.168404344971005170E-16, -1.203141491611682442E-30 ) ) ;
#7506 = AXIS2_PLACEMENT_3D ( 'NONE', #15836, #17974, #1842 ) ;
#7507 = CARTESIAN_POINT ( 'NONE',  ( 2.918498775983380256E-10, -9.961476088449217059E-10, -45.00000000000000000 ) ) ;
#7508 = CARTESIAN_POINT ( 'NONE',  ( 4.055487192203222513, 1.409979666030580114, -3.568038521265891827 ) ) ;
#7509 = ORIENTED_EDGE ( 'NONE', *, *, #2195, .F. ) ;
#7510 = DIRECTION ( 'NONE',  ( 0.000000000000000000, 1.000000000000000000, 0.000000000000000000 ) ) ;
#7511 = ADVANCED_FACE ( 'NONE', ( #11363 ), #19972, .F. ) ;
#7512 = ADVANCED_FACE ( 'NONE', ( #15014, #6085, #13031 ), #334, .T. ) ;
#7513 = PLANE ( 'NONE',  #9463 ) ;
#7514 = VERTEX_POINT ( 'NONE', #9735 ) ;
#7515 = AXIS2_PLACEMENT_3D ( 'NONE', #13932, #10526, #12515 ) ;
#7516 = CARTESIAN_POINT ( 'NONE',  ( -0.5000000000000559552, -2.000000000000029310, 8.000000000000062172 ) ) ;
#7517 = CARTESIAN_POINT ( 'NONE',  ( -55.05572809000118184, -2.700000000000125855, -8.000000000000062172 ) ) ;
#7518 = CARTESIAN_POINT ( 'NONE',  ( 3.974175853610027342, -2.726149789692876801, -2.409821656223177566 ) ) ;
#7519 = DIRECTION ( 'NONE',  ( -9.693457064947022734E-26, 0.000000000000000000, 1.000000000000000000 ) ) ;
#7520 = CARTESIAN_POINT ( 'NONE',  ( -1.040834085586084257E-13, 4.862606272033151100, -3.745885042887441063 ) ) ;
#7521 = CARTESIAN_POINT ( 'NONE',  ( 108.2426266706970637, -10.52760560296359138, 5.999999999999984901 ) ) ;
#7522 = CARTESIAN_POINT ( 'NONE',  ( -6.000000000000116351, -7.500000000000027534, -8.000000000000007105 ) ) ;
#7523 = B_SPLINE_CURVE_WITH_KNOTS ( 'NONE', 3,
 ( #17248, #18798, #15139, #9745, #17010 ),
 .UNSPECIFIED., .F., .F.,
 ( 4, 1, 4 ),
 ( 0.000000000000000000, 0.002020725942163689639, 0.004041451884327379278 ),
 .UNSPECIFIED. ) ;
#7524 = CARTESIAN_POINT ( 'NONE',  ( -2.775557561562891351E-14, 10.74999999999998579, -2.566987298107781257 ) ) ;
#7525 = ADVANCED_FACE ( 'NONE', ( #13151 ), #9388, .T. ) ;
#7526 = DIRECTION ( 'NONE',  ( 3.885780586188016830E-16, 4.437342591868156373E-31, -1.000000000000000000 ) ) ;
#7527 = CARTESIAN_POINT ( 'NONE',  ( 8.148407558030035247, -13.43987109532831070, 7.382406087064103950 ) ) ;
#7528 = CARTESIAN_POINT ( 'NONE',  ( 0.000000000000000000, -3.031088913245536087, -1.749999999999996447 ) ) ;
#7529 = EDGE_CURVE ( 'NONE', #6413, #10566, #1828, .T. ) ;
#7530 = CARTESIAN_POINT ( 'NONE',  ( 6.500000000000227374, 3.000000000000197176, 6.000000000000213163 ) ) ;
#7531 = DIRECTION ( 'NONE',  ( -0.5000000000000024425, 0.8660254037844372643, 0.000000000000000000 ) ) ;
#7533 = EDGE_CURVE ( 'NONE', #16514, #10858, #7465, .T. ) ;
#7532 = LINE ( 'NONE', #5771, #21657 ) ;
#7534 = CARTESIAN_POINT ( 'NONE',  ( 4.180231891692617552, -2.049421325483212986, -3.591231015387279069 ) ) ;
#7535 = VECTOR ( 'NONE', #16356, 1000.000000000000000 ) ;
#7536 = PRODUCT_CONTEXT ( 'NONE', #17783, 'mechanical' ) ;
#7537 = B_SPLINE_CURVE_WITH_KNOTS ( 'NONE', 3,
 ( #23140, #14187, #1824, #10302, #17952, #5366, #5255, #1376, #13942, #12525, #16047, #17472, #23259, #8542, #15702, #6774, #5002, #19360 ),
 .UNSPECIFIED., .F., .F.,
 ( 4, 2, 2, 2, 2, 2, 2, 2, 4 ),
 ( 0.000000000000000000, 0.0005979442104825548809, 0.001195888420965109762, 0.001793832631447664534, 0.002391776841930219524, 0.002989721052412774513, 0.003587665262895329069, 0.004185609473377884492, 0.004783553683860439047 ),
 .UNSPECIFIED. ) ;
#7538 = ORIENTED_EDGE ( 'NONE', *, *, #22942, .T. ) ;
#7539 = EDGE_CURVE ( 'NONE', #7229, #1035, #21854, .T. ) ;
#7541 = ORIENTED_EDGE ( 'NONE', *, *, #21078, .F. ) ;
#7540 = ORIENTED_EDGE ( 'NONE', *, *, #19570, .T. ) ;
#7542 = FACE_OUTER_BOUND ( 'NONE', #7194, .T. ) ;
#7543 = DIRECTION ( 'NONE',  ( 0.000000000000000000, 1.000000000000000000, 0.000000000000000000 ) ) ;
#7544 = CARTESIAN_POINT ( 'NONE',  ( -47.82842712474641189, -4.371572875253856516, 7.500000000000047962 ) ) ;
#7545 = ORIENTED_EDGE ( 'NONE', *, *, #11685, .T. ) ;
#7546 = CIRCLE ( 'NONE', #1908, 0.4999999999999978351 ) ;
#7547 = CARTESIAN_POINT ( 'NONE',  ( 4.170895651974840135, 4.109780709045198321, 2.116862463031252292E-13 ) ) ;
#7548 = EDGE_CURVE ( 'NONE', #2913, #14457, #11143, .T. ) ;
#7549 = CARTESIAN_POINT ( 'NONE',  ( -43.10883117545719045, 7.499999999999992895, 7.500000000000007105 ) ) ;
#7550 = CARTESIAN_POINT ( 'NONE',  ( -12.84999999999999964, -6.938893903907228378E-15, 5.749999999999991118 ) ) ;
#7551 = DIRECTION ( 'NONE',  ( 1.000000000000000000, 2.220446049250314067E-16, -5.825996348268307008E-33 ) ) ;
#7552 = CARTESIAN_POINT ( 'NONE',  ( 124.5000000000017195, -4.000000000000058620, 1.387778780781445676E-14 ) ) ;
#7553 = DIRECTION ( 'NONE',  ( 1.000000000000000000, -1.276756478318923119E-15, 1.387778780781436998E-15 ) ) ;
#7554 = CARTESIAN_POINT ( 'NONE',  ( -2.081668171172168513E-14, 4.250000000000003553, -1.250000000000001110 ) ) ;
#7555 = FACE_OUTER_BOUND ( 'NONE', #3387, .T. ) ;
#7556 = CARTESIAN_POINT ( 'NONE',  ( 22.49999999999994671, 4.500000000000059508, -18.74999999999998224 ) ) ;
#7557 = DIRECTION ( 'NONE',  ( 1.066786462891689527E-26, 6.656013887802287108E-31, 1.000000000000000000 ) ) ;
#7558 = FACE_OUTER_BOUND ( 'NONE', #21590, .T. ) ;
#7559 = CARTESIAN_POINT ( 'NONE',  ( 6.000000000291855429, -0.5000000009961480529, -8.549999999999998934 ) ) ;
#7560 = PLANE ( 'NONE',  #692 ) ;
#7561 = CARTESIAN_POINT ( 'NONE',  ( 7.479729963966237349, -0.8034648269415383126, 9.265052153039572858 ) ) ;
#7562 = ORIENTED_EDGE ( 'NONE', *, *, #6970, .T. ) ;
#7563 = CIRCLE ( 'NONE', #20343, 4.000000000000023981 ) ;
#7564 = AXIS2_PLACEMENT_3D ( 'NONE', #4416, #17234, #15470 ) ;
#7566 = ORIENTED_EDGE ( 'NONE', *, *, #5746, .T. ) ;
#7565 = ORIENTED_EDGE ( 'NONE', *, *, #2207, .T. ) ;
#7567 = B_SPLINE_CURVE_WITH_KNOTS ( 'NONE', 3,
 ( #15521, #8590, #13771, #15287, #6829, #18951, #22481, #3190 ),
 .UNSPECIFIED., .F., .F.,
 ( 4, 2, 2, 4 ),
 ( 0.002775112046897012467, 0.003466237704215415199, 0.004157363361533817497, 0.005539614676170622962 ),
 .UNSPECIFIED. ) ;
#7568 = VERTEX_POINT ( 'NONE', #7619 ) ;
#7570 = VERTEX_POINT ( 'NONE', #14792 ) ;
#7569 = ORIENTED_EDGE ( 'NONE', *, *, #10869, .F. ) ;
#7571 = ORIENTED_EDGE ( 'NONE', *, *, #13581, .F. ) ;
#7572 = CARTESIAN_POINT ( 'NONE',  ( 0.1217565302851104925, 2.351289329882151335, 2.927447417349534842 ) ) ;
#7573 = ORIENTED_EDGE ( 'NONE', *, *, #11395, .F. ) ;
#7574 = VERTEX_POINT ( 'NONE', #2315 ) ;
#7575 = EDGE_CURVE ( 'NONE', #888, #8962, #20999, .T. ) ;
#7576 = CARTESIAN_POINT ( 'NONE',  ( 2.918498775983380256E-10, 6.999999999003851947, -15.99999999999999289 ) ) ;
#7577 = CARTESIAN_POINT ( 'NONE',  ( -2.000000000000043077, -3.464101615137785917, -3.142992957459260772 ) ) ;
#7578 = ADVANCED_FACE ( 'NONE', ( #18436 ), #9495, .T. ) ;
#7579 = CARTESIAN_POINT ( 'NONE',  ( 37.86602540378459025, -1.387778780781445676E-14, -2.133974596215476360 ) ) ;
#7580 = CARTESIAN_POINT ( 'NONE',  ( -7.024848138040975520, -2.659619850263430507, 8.468562630484278486 ) ) ;
#7581 = FACE_OUTER_BOUND ( 'NONE', #13950, .T. ) ;
#7582 = DIRECTION ( 'NONE',  ( -0.7071067811865491270, -0.7071067811865461294, -1.565905175853767167E-16 ) ) ;
#7583 = AXIS2_PLACEMENT_3D ( 'NONE', #4413, #7840, #15007 ) ;
#7584 = DIRECTION ( 'NONE',  ( 0.000000000000000000, 0.000000000000000000, 1.000000000000000000 ) ) ;
#7585 = DIRECTION ( 'NONE',  ( 2.013525853228507892E-32, 6.902532920683810383E-31, -1.000000000000000000 ) ) ;
#7586 = EDGE_CURVE ( 'NONE', #9423, #6499, #715, .T. ) ;
#7587 = DIRECTION ( 'NONE',  ( 1.000000000000000000, 1.479114197289397135E-31, 5.916456789157588541E-31 ) ) ;
#7588 = LINE ( 'NONE', #1933, #23185 ) ;
#7589 = ORIENTED_EDGE ( 'NONE', *, *, #18556, .F. ) ;
#7590 = SURFACE_STYLE_USAGE ( .BOTH. , #16288 ) ;
#7591 = DIRECTION ( 'NONE',  ( 1.000000000000000000, 0.000000000000000000, 0.000000000000000000 ) ) ;
#7593 = ORIENTED_EDGE ( 'NONE', *, *, #325, .F. ) ;
#7592 = ORIENTED_EDGE ( 'NONE', *, *, #21065, .F. ) ;
#7594 = ORIENTED_EDGE ( 'NONE', *, *, #14038, .T. ) ;
#7595 = EDGE_LOOP ( 'NONE', ( #6465, #19424, #7482, #15236 ) ) ;
#7596 = AXIS2_PLACEMENT_3D ( 'NONE', #9434, #17170, #2596 ) ;
#7597 = AXIS2_PLACEMENT_3D ( 'NONE', #4292, #18776, #11469 ) ;
#7598 = CIRCLE ( 'NONE', #14727, 0.5155456020628804703 ) ;
#7599 = ORIENTED_EDGE ( 'NONE', *, *, #22939, .F. ) ;
#7600 = ORIENTED_EDGE ( 'NONE', *, *, #19893, .T. ) ;
#7601 = FACE_OUTER_BOUND ( 'NONE', #18072, .T. ) ;
#7602 = CARTESIAN_POINT ( 'NONE',  ( 4.142654963991861727, -4.070796997468701051, 2.081660976370999833E-14 ) ) ;
#7603 = CARTESIAN_POINT ( 'NONE',  ( 0.000000000000000000, 10.49999999999999822, -10.86602540378443749 ) ) ;
#7604 = CYLINDRICAL_SURFACE ( 'NONE', #3360, 2.549999999999997158 ) ;
#7605 = CARTESIAN_POINT ( 'NONE',  ( -6.938893903907228378E-14, 4.999999999999976907, -4.163336342344337027E-14 ) ) ;
#7606 = LINE ( 'NONE', #5504, #22406 ) ;
#7607 =( BOUNDED_SURFACE ( )  B_SPLINE_SURFACE ( 3, 2, ( 
 ( #13702, #6294, #4389 ),
 ( #20879, #11571, #7821 ),
 ( #17089, #4628, #10048 ),
 ( #4747, #10162, #20649 ),
 ( #11916, #2750, #8168 ),
 ( #4517, #14987, #15335 ) ),
 .UNSPECIFIED., .F., .F., .F. ) 
 B_SPLINE_SURFACE_WITH_KNOTS ( ( 4, 2, 4 ),
 ( 3, 3 ),
 ( 0.01652267773200354062, 0.01858309280828998253, 0.02064350788457642444 ),
 ( 0.000000000000000000, 1.000000000000000000 ),
 .UNSPECIFIED. ) 
 GEOMETRIC_REPRESENTATION_ITEM ( )  RATIONAL_B_SPLINE_SURFACE ( (
 ( 1.000000000000000000, 0.8047780975688280103, 1.000000000000000000),
 ( 1.000000000000000000, 0.8123789546318919141, 1.000000000000000000),
 ( 1.000000000000000000, 0.8190677982996300566, 1.000000000000000000),
 ( 1.000000000000000000, 0.8192346069544601539, 1.000000000000000000),
 ( 1.000000000000000000, 0.8126126759774594532, 1.000000000000000000),
 ( 1.000000000000000000, 0.8047712639312011307, 1.000000000000000000) ) ) 
 REPRESENTATION_ITEM ( '' )  SURFACE ( )  );
#7608 = DIRECTION ( 'NONE',  ( -1.000000000000000000, -2.220446049250301001E-16, 0.000000000000000000 ) ) ;
#7609 = CARTESIAN_POINT ( 'NONE',  ( -3.610629513653773603, 4.785505255291086613, -7.500000000000001776 ) ) ;
#7610 = STYLED_ITEM ( 'NONE', ( #12761 ), #5189 ) ;
#7611 = AXIS2_PLACEMENT_3D ( 'NONE', #12400, #1819, #19582 ) ;
#7612 = DIRECTION ( 'NONE',  ( 1.134196829589822256E-15, 2.220446049250322449E-16, -1.000000000000000000 ) ) ;
#7613 = VECTOR ( 'NONE', #21730, 1000.000000000000000 ) ;
#7614 = CARTESIAN_POINT ( 'NONE',  ( -4.346882592290722158, 1.739972214219213331, -1.970978495615576698 ) ) ;
#7615 = AXIS2_PLACEMENT_3D ( 'NONE', #13217, #4268, #11446 ) ;
#7616 = VECTOR ( 'NONE', #634, 1000.000000000000000 ) ;
#7617 = PRODUCT_DEFINITION ( 'UNKNOWN', '', #21044, #20651 ) ;
#7618 = FILL_AREA_STYLE ('',( #13150 ) ) ;
#7619 = CARTESIAN_POINT ( 'NONE',  ( -1.365901330155232488E-14, -24.99999999999998579, 7.882182279042429407 ) ) ;
#7620 = CARTESIAN_POINT ( 'NONE',  ( 4.180345136606689493, -2.085999704580133507, -3.570468642550126415 ) ) ;
#7621 = ADVANCED_FACE ( 'NONE', ( #2666 ), #12411, .F. ) ;
#7622 = VERTEX_POINT ( 'NONE', #8314 ) ;
#7623 = CARTESIAN_POINT ( 'NONE',  ( -6.649675532656710075, 36.01889503913412227, -27.42797899728712352 ) ) ;
#7624 = DIRECTION ( 'NONE',  ( 0.000000000000000000, 0.000000000000000000, 1.000000000000000000 ) ) ;
#7625 = AXIS2_PLACEMENT_3D ( 'NONE', #6770, #19357, #20793 ) ;
#7627 = EDGE_CURVE ( 'NONE', #1330, #21815, #17899, .T. ) ;
#7626 = VERTEX_POINT ( 'NONE', #10186 ) ;
#7628 = VECTOR ( 'NONE', #1557, 1000.000000000000000 ) ;
#7629 = PLANE ( 'NONE',  #8780 ) ;
#7630 = AXIS2_PLACEMENT_3D ( 'NONE', #16271, #408, #9345 ) ;
#7631 = CIRCLE ( 'NONE', #8392, 0.4999999999999999445 ) ;
#7632 = CARTESIAN_POINT ( 'NONE',  ( -1.318516776095816523, -3.857556137907097060, -5.599999999999981881 ) ) ;
#7633 = DIRECTION ( 'NONE',  ( 0.5000000000000003331, 0.000000000000000000, 0.8660254037844384856 ) ) ;
#7634 = CYLINDRICAL_SURFACE ( 'NONE', #6023, 6.000000000000047073 ) ;
#7635 = CARTESIAN_POINT ( 'NONE',  ( -3.336453936897187944, 0.5000000000000628386, -21.17547853860574136 ) ) ;
#7636 = DIRECTION ( 'NONE',  ( 0.000000000000000000, 0.000000000000000000, 1.000000000000000000 ) ) ;
#7637 = DIRECTION ( 'NONE',  ( 1.479114197289397135E-31, -1.000000000000000000, 3.382522293539642681E-32 ) ) ;
#7638 = DIRECTION ( 'NONE',  ( 1.000000000000000000, 0.000000000000000000, 0.000000000000000000 ) ) ;
#7639 = LINE ( 'NONE', #18456, #19332 ) ;
#7640 = DIRECTION ( 'NONE',  ( -1.815210279346896549E-30, 6.902532920684321857E-31, -1.000000000000000000 ) ) ;
#7641 = DIRECTION ( 'NONE',  ( -2.013525853228518840E-32, 6.902532920683810383E-31, -1.000000000000000000 ) ) ;
#7642 = DIRECTION ( 'NONE',  ( 0.000000000000000000, -4.190823558986609452E-31, 1.000000000000000000 ) ) ;
#7643 = EDGE_CURVE ( 'NONE', #22557, #145, #3021, .T. ) ;
#7644 = CONICAL_SURFACE ( 'NONE', #18917, 4.750000000000000000, 1.047197551196600074 ) ;
#7645 = FACE_BOUND ( 'NONE', #12325, .T. ) ;
#7646 = CONICAL_SURFACE ( 'NONE', #2755, 3.499999999999999556, 1.047197551196600074 ) ;
#7647 = AXIS2_PLACEMENT_3D ( 'NONE', #22747, #8400, #21228 ) ;
#7649 = EDGE_CURVE ( 'NONE', #8523, #16088, #15130, .T. ) ;
#7648 = CIRCLE ( 'NONE', #12529, 0.5000000000000038858 ) ;
#7650 = AXIS2_PLACEMENT_3D ( 'NONE', #8729, #8499, #6983 ) ;
#7651 = CONTEXT_DEPENDENT_SHAPE_REPRESENTATION ( #5030, #1039 ) ;
#7652 = VERTEX_POINT ( 'NONE', #15363 ) ;
#7655 = ORIENTED_EDGE ( 'NONE', *, *, #3221, .T. ) ;
#7654 = EDGE_CURVE ( 'NONE', #4543, #10008, #4667, .T. ) ;
#7653 = ORIENTED_EDGE ( 'NONE', *, *, #5357, .T. ) ;
#7656 = ADVANCED_FACE ( 'NONE', ( #18909 ), #13376, .T. ) ;
#7657 = DIRECTION ( 'NONE',  ( -1.000000000000000000, -1.110223024625164429E-16, -2.013525853228515555E-32 ) ) ;
#7658 = CARTESIAN_POINT ( 'NONE',  ( 7.332081355611481222, -0.2267865287842198430, 7.890992604157067269 ) ) ;
#7659 = CARTESIAN_POINT ( 'NONE',  ( 2.918498775983380256E-10, 2.999999999003851503, -45.00000000000000000 ) ) ;
#7660 = VECTOR ( 'NONE', #18902, 1000.000000000000000 ) ;
#7661 = ORIENTED_EDGE ( 'NONE', *, *, #2788, .F. ) ;
#7662 = CONICAL_SURFACE ( 'NONE', #20835, 3.500000000000004441, 1.047197551196600296 ) ;
#7663 = CARTESIAN_POINT ( 'NONE',  ( 4.124214193018068464, 4.056676826581881556, 3.377256047658116025E-15 ) ) ;
#7664 = DIRECTION ( 'NONE',  ( -3.254448077146059901E-32, -1.000000000000000000, 6.656013887802287108E-31 ) ) ;
#7665 = AXIS2_PLACEMENT_3D ( 'NONE', #807, #11958, #1273 ) ;
#7666 = CARTESIAN_POINT ( 'NONE',  ( 7.500000000000007105, -8.000000000000003553, 12.24999999999999645 ) ) ;
#7667 = CARTESIAN_POINT ( 'NONE',  ( 1.031902578047550589, -0.5999999999999896527, -4.508672757499345707 ) ) ;
#7668 = SURFACE_STYLE_USAGE ( .BOTH. , #495 ) ;
#7669 = DIRECTION ( 'NONE',  ( 0.7071067811865485719, -0.7071067811865463515, -1.010793663541191485E-16 ) ) ;
#7670 = DIRECTION ( 'NONE',  ( -7.395570986446975166E-31, -3.382522293539642681E-32, -1.000000000000000000 ) ) ;
#7671 = LINE ( 'NONE', #12965, #9877 ) ;
#7672 = DIRECTION ( 'NONE',  ( 0.8191520442889970166, -9.614764631795313332E-16, -0.5735764363510387209 ) ) ;
#7673 = EDGE_CURVE ( 'NONE', #7463, #12394, #11840, .T. ) ;
#7675 = EDGE_CURVE ( 'NONE', #6667, #5868, #19889, .T. ) ;
#7674 = FACE_OUTER_BOUND ( 'NONE', #5405, .T. ) ;
#7676 = EDGE_CURVE ( 'NONE', #13819, #19925, #13491, .T. ) ;
#7677 = DIRECTION ( 'NONE',  ( 2.013525853228507892E-32, 6.902532920683810383E-31, -1.000000000000000000 ) ) ;
#7678 = DIRECTION ( 'NONE',  ( -5.551115123561405253E-17, -1.000000000000000000, -2.256980353643891447E-27 ) ) ;
#7679 = CARTESIAN_POINT ( 'NONE',  ( 7.132286784435700078, -0.4236497315830464183, 8.470912490188409194 ) ) ;
#7680 = ORIENTED_EDGE ( 'NONE', *, *, #21339, .F. ) ;
#7681 = TOROIDAL_SURFACE ( 'NONE', #10310, 6.500000000000000888, 0.5000000000000000000 ) ;
#7682 = AXIS2_PLACEMENT_3D ( 'NONE', #3426, #9058, #17890 ) ;
#7684 = VERTEX_POINT ( 'NONE', #22433 ) ;
#7683 = ORIENTED_EDGE ( 'NONE', *, *, #12856, .F. ) ;
#7685 = UNCERTAINTY_MEASURE_WITH_UNIT (LENGTH_MEASURE( 1.000000000000000082E-05 ), #3474, 'distance_accuracy_value', 'NONE');
#7686 = ADVANCED_FACE ( 'NONE', ( #10082 ), #20911, .T. ) ;
#7687 = AXIS2_PLACEMENT_3D ( 'NONE', #9719, #783, #7944 ) ;
#7688 = ORIENTED_EDGE ( 'NONE', *, *, #17678, .T. ) ;
#7691 = EDGE_LOOP ( 'NONE', ( #13301, #13954 ) ) ;
#7690 = EDGE_CURVE ( 'NONE', #6390, #16034, #13497, .T. ) ;
#7689 = VERTEX_POINT ( 'NONE', #19240 ) ;
#7692 = VERTEX_POINT ( 'NONE', #2790 ) ;
#7693 = CARTESIAN_POINT ( 'NONE',  ( 0.4500000002918510544, 42.99999999900385461, -29.00000000000000355 ) ) ;
#7694 = VERTEX_POINT ( 'NONE', #6905 ) ;
#7695 = ORIENTED_EDGE ( 'NONE', *, *, #1268, .F. ) ;
#7696 = LINE ( 'NONE', #19938, #9548 ) ;
#7697 = CARTESIAN_POINT ( 'NONE',  ( -6.000000000000088818, -2.000000000000050182, -17.72029585817572084 ) ) ;
#7698 = CARTESIAN_POINT ( 'NONE',  ( -1.387778780781445676E-14, -24.99999999999998224, 0.000000000000000000 ) ) ;
#7699 = DIRECTION ( 'NONE',  ( -1.550910762415566494E-16, -1.000000000000000000, 8.135128085091684243E-31 ) ) ;
#7700 = LINE ( 'NONE', #18285, #19258 ) ;
#7701 =( GEOMETRIC_REPRESENTATION_CONTEXT ( 3 ) GLOBAL_UNCERTAINTY_ASSIGNED_CONTEXT ( ( #629 ) ) GLOBAL_UNIT_ASSIGNED_CONTEXT ( ( #16359, #4348, #5680 ) ) REPRESENTATION_CONTEXT ( 'NONE', 'WORKASPACE' ) );
#7702 = CARTESIAN_POINT ( 'NONE',  ( -3.510273485745384558, -2.827716139362705938, -3.610536846335915317 ) ) ;
#7703 = CARTESIAN_POINT ( 'NONE',  ( 2.775557561562891351E-14, 8.000000000000003553, -6.499999999999950262 ) ) ;
#7704 = FACE_OUTER_BOUND ( 'NONE', #22535, .T. ) ;
#7705 = CARTESIAN_POINT ( 'NONE',  ( 37.36637401601559105, 10.68627026436968386, -2.633625983984380081 ) ) ;
#7706 = ORIENTED_EDGE ( 'NONE', *, *, #1025, .T. ) ;
#7707 = UNCERTAINTY_MEASURE_WITH_UNIT (LENGTH_MEASURE( 1.000000000000000082E-05 ), #8490, 'distance_accuracy_value', 'NONE');
#7708 = DIRECTION ( 'NONE',  ( 1.000000000000000000, 2.220446049250313081E-16, 4.712618736834399899E-47 ) ) ;
#7710 = VERTEX_POINT ( 'NONE', #1598 ) ;
#7709 = VERTEX_POINT ( 'NONE', #7027 ) ;
#7711 = ADVANCED_FACE ( 'NONE', ( #3601 ), #7253, .T. ) ;
#7712 = VERTEX_POINT ( 'NONE', #5258 ) ;
#7713 = AXIS2_PLACEMENT_3D ( 'NONE', #22809, #20465, #17027 ) ;
#7714 = ORIENTED_EDGE ( 'NONE', *, *, #19578, .T. ) ;
#7715 = EDGE_LOOP ( 'NONE', ( #13706, #16061, #17246, #4033 ) ) ;
#7716 = EDGE_CURVE ( 'NONE', #19728, #11543, #9746, .T. ) ;
#7717 = DIRECTION ( 'NONE',  ( 0.000000000000000000, 0.000000000000000000, 1.000000000000000000 ) ) ;
#7718 = CARTESIAN_POINT ( 'NONE',  ( -42.54314575050795355, 3.999999999999996447, -7.500000000000007105 ) ) ;
#7719 = ORIENTED_EDGE ( 'NONE', *, *, #18361, .T. ) ;
#7720 = PLANE ( 'NONE',  #20373 ) ;
#7721 = CARTESIAN_POINT ( 'NONE',  ( 86.00000000000117950, -10.52760560296347947, 6.000000000000054179 ) ) ;
#7722 = FACE_OUTER_BOUND ( 'NONE', #12118, .T. ) ;
#7723 = B_SPLINE_CURVE_WITH_KNOTS ( 'NONE', 3,
 ( #5416, #17511, #16091, #12449, #1748, #7296, #5170, #12210 ),
 .UNSPECIFIED., .F., .F.,
 ( 4, 2, 2, 4 ),
 ( 0.002775112046897004661, 0.003466237704215408694, 0.004157363361533812293, 0.005539614676170621227 ),
 .UNSPECIFIED. ) ;
#7724 = CARTESIAN_POINT ( 'NONE',  ( -6.999999999708142795, 38.99999999900385461, -26.00000000000000000 ) ) ;
#7725 = CARTESIAN_POINT ( 'NONE',  ( 4.093692494532772841, 4.043567292011542413, 4.394662665088411898E-17 ) ) ;
#7726 = CARTESIAN_POINT ( 'NONE',  ( 6.999999999999978684, -8.000000000000017764, 10.24999999999998224 ) ) ;
#7727 = CARTESIAN_POINT ( 'NONE',  ( -4.330127018922234505, 4.689110867544671102, -7.500000000000000000 ) ) ;
#7728 = EDGE_CURVE ( 'NONE', #15995, #10242, #10113, .T. ) ;
#7729 = FACE_OUTER_BOUND ( 'NONE', #7320, .T. ) ;
#7730 = FACE_BOUND ( 'NONE', #8941, .T. ) ;
#7731 = VECTOR ( 'NONE', #14144, 1000.000000000000000 ) ;
#7732 = DIRECTION ( 'NONE',  ( -0.000000000000000000, -0.000000000000000000, 1.000000000000000000 ) ) ;
#7733 = CARTESIAN_POINT ( 'NONE',  ( -6.962001439796708269, 35.99999999900384751, -26.47597002942762145 ) ) ;
#7734 = ORIENTED_EDGE ( 'NONE', *, *, #11395, .T. ) ;
#7735 = VECTOR ( 'NONE', #20441, 1000.000000000000000 ) ;
#7736 = ORIENTED_EDGE ( 'NONE', *, *, #3866, .F. ) ;
#7737 = CARTESIAN_POINT ( 'NONE',  ( -87.15000000000065938, 3.200000000000057465, -2.000000000000001332 ) ) ;
#7738 = DIRECTION ( 'NONE',  ( -1.066788928082016908E-26, -3.471809175856251779E-58, 1.000000000000000000 ) ) ;
#7739 = ORIENTED_EDGE ( 'NONE', *, *, #5645, .T. ) ;
#7740 = AXIS2_PLACEMENT_3D ( 'NONE', #9379, #16527, #18088 ) ;
#7741 = DIRECTION ( 'NONE',  ( 2.013525853228518840E-32, -6.902532920683810383E-31, 1.000000000000000000 ) ) ;
#7742 = CARTESIAN_POINT ( 'NONE',  ( 0.000000000000000000, 1.387778780781445676E-14, -10.86602540378443749 ) ) ;
#7743 = CARTESIAN_POINT ( 'NONE',  ( 108.2426266706970637, -6.527605602963671316, -5.999999999999991118 ) ) ;
#7744 = CARTESIAN_POINT ( 'NONE',  ( 1.387778780781445676E-14, 4.163336342344337027E-14, -2.000000000000001776 ) ) ;
#7745 = CIRCLE ( 'NONE', #619, 4.749999999999986677 ) ;
#7746 = PLANE ( 'NONE',  #12154 ) ;
#7747 = DIRECTION ( 'NONE',  ( -1.000000000000000000, -1.910522504832140594E-31, 5.551115123125818447E-17 ) ) ;
#7748 = EDGE_LOOP ( 'NONE', ( #23241, #2613, #18390, #10774 ) ) ;
#7749 = FACE_OUTER_BOUND ( 'NONE', #16800, .T. ) ;
#7750 = LINE ( 'NONE', #13170, #12524 ) ;
#7751 = AXIS2_PLACEMENT_3D ( 'NONE', #4049, #14756, #19948 ) ;
#7752 = ADVANCED_FACE ( 'NONE', ( #7148 ), #4457, .T. ) ;
#7753 = CARTESIAN_POINT ( 'NONE',  ( 2.789435349370705492E-14, 11.99999999999999645, -2.499999999999987121 ) ) ;
#7754 = DIRECTION ( 'NONE',  ( -1.000000000000000000, -1.734723475976799009E-15, -9.165585228034679171E-32 ) ) ;
#7755 = CARTESIAN_POINT ( 'NONE',  ( -45.01801948466079040, -6.474873734152946092, 8.000000000000021316 ) ) ;
#7756 = DIRECTION ( 'NONE',  ( -9.693457064947022734E-26, 0.000000000000000000, 1.000000000000000000 ) ) ;
#7757 = CARTESIAN_POINT ( 'NONE',  ( 4.180345304246198879, -4.135116856707397481, 0.02129519942689462111 ) ) ;
#7758 = TOROIDAL_SURFACE ( 'NONE', #2128, 5.750000000000000000, 0.5000000000000000000 ) ;
#7759 = ITEM_DEFINED_TRANSFORMATION ( 'NONE', 'NONE', #16500,  #22115 ) ;
#7760 = ORIENTED_EDGE ( 'NONE', *, *, #3171, .T. ) ;
#7761 = EDGE_CURVE ( 'NONE', #2264, #12125, #17958, .T. ) ;
#7763 = ORIENTED_EDGE ( 'NONE', *, *, #1878, .T. ) ;
#7762 = ORIENTED_EDGE ( 'NONE', *, *, #11839, .T. ) ;
#7764 = CARTESIAN_POINT ( 'NONE',  ( 2.499999999999992006, 2.000000000000001776, -1.250000000000028866 ) ) ;
#7765 = CARTESIAN_POINT ( 'NONE',  ( 37.77870956205638464, -7.009096939670001340E-15, -2.308606279672925865 ) ) ;
#7766 = EDGE_CURVE ( 'NONE', #22878, #12541, #19833, .T. ) ;
#7767 = SURFACE_STYLE_FILL_AREA ( #9651 ) ;
#7768 = ORIENTED_EDGE ( 'NONE', *, *, #14555, .T. ) ;
#7769 = DIRECTION ( 'NONE',  ( 0.000000000000000000, 0.000000000000000000, -1.000000000000000000 ) ) ;
#7770 = DIRECTION ( 'NONE',  ( 0.000000000000000000, 1.000000000000000000, 0.000000000000000000 ) ) ;
#7771 = DIRECTION ( 'NONE',  ( 1.333893503340774882E-15, 2.778352770573747380E-17, 1.000000000000000000 ) ) ;
#7772 = EDGE_CURVE ( 'NONE', #16593, #1206, #21137, .T. ) ;
#7773 = CARTESIAN_POINT ( 'NONE',  ( 0.4427966827908824676, -0.5999999999999897637, -4.147834322102026405 ) ) ;
#7774 = DIRECTION ( 'NONE',  ( 0.000000000000000000, 0.000000000000000000, 1.000000000000000000 ) ) ;
#7775 = CARTESIAN_POINT ( 'NONE',  ( 4.000000000000003553, 2.309401076758525573, -5.242734410091827613 ) ) ;
#7776 = CARTESIAN_POINT ( 'NONE',  ( 5.089746846163173136E-15, 3.025336207442039000E-31, -4.487534009422209813 ) ) ;
#7777 = DIRECTION ( 'NONE',  ( -0.6819983600624998088, -0.7313537016191693496, 0.000000000000000000 ) ) ;
#7778 = CARTESIAN_POINT ( 'NONE',  ( -12.85000000000004228, -1.499999999999997780, -6.249999999999977796 ) ) ;
#7779 = B_SPLINE_CURVE_WITH_KNOTS ( 'NONE', 3,
 ( #16366, #268, #11077, #2135, #14616, #3450, #21804, #5686, #10617, #21462, #5331, #17922, #4129, #18382 ),
 .UNSPECIFIED., .F., .F.,
 ( 4, 2, 2, 2, 2, 2, 4 ),
 ( 0.000000000000000000, 0.0004465115319127612543, 0.0008930230638255225086, 0.001339534595738283871, 0.001786046127651045017, 0.002679069191476569911, 0.003572092255302094805 ),
 .UNSPECIFIED. ) ;
#7780 = VECTOR ( 'NONE', #11306, 1000.000000000000000 ) ;
#7781 = AXIS2_PLACEMENT_3D ( 'NONE', #15991, #19652, #12348 ) ;
#7782 = EDGE_CURVE ( 'NONE', #635, #17483, #21400, .T. ) ;
#7783 = CARTESIAN_POINT ( 'NONE',  ( 7.499999999999992895, -5.999999999999981348, 6.250000000000005329 ) ) ;
#7784 = DIRECTION ( 'NONE',  ( 1.000000000000000000, -2.168404344971005170E-16, 1.203141491611682442E-30 ) ) ;
#7785 = EDGE_CURVE ( 'NONE', #3913, #6272, #341, .T. ) ;
#7786 = PLANE ( 'NONE',  #10457 ) ;
#7787 = CARTESIAN_POINT ( 'NONE',  ( -3.999999999708153453, 42.99999999900385461, -15.99999999999999289 ) ) ;
#7788 = ADVANCED_FACE ( 'NONE', ( #10880 ), #11595, .T. ) ;
#7789 = ORIENTED_EDGE ( 'NONE', *, *, #8205, .F. ) ;
#7790 = AXIS2_PLACEMENT_3D ( 'NONE', #13348, #13577, #20530 ) ;
#7792 = ORIENTED_EDGE ( 'NONE', *, *, #18954, .T. ) ;
#7791 = ORIENTED_EDGE ( 'NONE', *, *, #9657, .T. ) ;
#7793 = VECTOR ( 'NONE', #998, 1000.000000000000000 ) ;
#7794 = VERTEX_POINT ( 'NONE', #3483 ) ;
#7795 = EDGE_LOOP ( 'NONE', ( #11989, #14879, #8875, #7565 ) ) ;
#7797 = ORIENTED_EDGE ( 'NONE', *, *, #2396, .T. ) ;
#7796 = ORIENTED_EDGE ( 'NONE', *, *, #9880, .T. ) ;
#7798 = AXIS2_PLACEMENT_3D ( 'NONE', #9634, #7754, #21877 ) ;
#7799 = ORIENTED_EDGE ( 'NONE', *, *, #6807, .T. ) ;
#7800 = DIRECTION ( 'NONE',  ( -1.000000000000000000, -2.168404344971017743E-16, 1.780660105995169760E-30 ) ) ;
#7801 = ADVANCED_FACE ( 'NONE', ( #3712 ), #19726, .T. ) ;
#7802 = AXIS2_PLACEMENT_3D ( 'NONE', #14557, #17625, #17742 ) ;
#7803 = VERTEX_POINT ( 'NONE', #5488 ) ;
#7804 = ORIENTED_EDGE ( 'NONE', *, *, #4874, .T. ) ;
#7805 = EDGE_CURVE ( 'NONE', #12275, #6044, #11980, .T. ) ;
#7806 = DIRECTION ( 'NONE',  ( 1.000000000000000000, 0.000000000000000000, 0.000000000000000000 ) ) ;
#7807 = CARTESIAN_POINT ( 'NONE',  ( 77.42435809754137210, -6.999999999999811706, 6.500000000000081712 ) ) ;
#7808 = DIRECTION ( 'NONE',  ( 1.000000000000000000, 1.479114197289387852E-30, -2.013525853228518840E-32 ) ) ;
#7809 = CIRCLE ( 'NONE', #20576, 2.550000000000010481 ) ;
#7810 = DIRECTION ( 'NONE',  ( 3.885780586188016830E-16, 4.437342591868156373E-31, -1.000000000000000000 ) ) ;
#7811 = CARTESIAN_POINT ( 'NONE',  ( -55.25320565519150051, 2.700000000000098321, 7.500000000000062172 ) ) ;
#7812 = STYLED_ITEM ( 'NONE', ( #22379 ), #6835 ) ;
#7813 = FACE_OUTER_BOUND ( 'NONE', #17928, .T. ) ;
#7814 = DIRECTION ( 'NONE',  ( 0.000000000000000000, -0.8381404052084435730, -0.5454545454545466354 ) ) ;
#7815 = CARTESIAN_POINT ( 'NONE',  ( 0.3126073911696447549, -4.041451884327432076, 3.469446951953614189E-15 ) ) ;
#7816 = EDGE_CURVE ( 'NONE', #22431, #22269, #12646, .T. ) ;
#7817 = DIRECTION ( 'NONE',  ( 1.000000000000000000, 3.254448077276381206E-32, 1.066788928082016908E-26 ) ) ;
#7818 = VECTOR ( 'NONE', #3681, 1000.000000000000000 ) ;
#7819 = CARTESIAN_POINT ( 'NONE',  ( 0.3126073911696447549, 2.020725942163625888, -3.499999999999996003 ) ) ;
#7820 = EDGE_CURVE ( 'NONE', #22329, #3406, #4847, .T. ) ;
#7821 = CARTESIAN_POINT ( 'NONE',  ( 4.055487192203090174, 1.409979666030529266, -3.568038521265504137 ) ) ;
#7822 = EDGE_CURVE ( 'NONE', #22156, #9451, #11717, .T. ) ;
#7823 = AXIS2_PLACEMENT_3D ( 'NONE', #14277, #17675, #12025 ) ;
#7824 = ORIENTED_EDGE ( 'NONE', *, *, #12263, .F. ) ;
#7825 =( LENGTH_UNIT ( ) NAMED_UNIT ( * ) SI_UNIT ( .MILLI., .METRE. ) );
#7827 = ORIENTED_EDGE ( 'NONE', *, *, #14716, .F. ) ;
#7826 = ORIENTED_EDGE ( 'NONE', *, *, #3551, .F. ) ;
#7828 = ORIENTED_EDGE ( 'NONE', *, *, #17867, .F. ) ;
#7829 = AXIS2_PLACEMENT_3D ( 'NONE', #1424, #8599, #15763 ) ;
#7830 = ORIENTED_EDGE ( 'NONE', *, *, #10067, .T. ) ;
#7831 = AXIS2_PLACEMENT_3D ( 'NONE', #6834, #20853, #4479 ) ;
#7832 = ORIENTED_EDGE ( 'NONE', *, *, #8474, .T. ) ;
#7833 = CARTESIAN_POINT ( 'NONE',  ( 4.158413352280815545, -2.044871626972879941, 3.541821552872997714 ) ) ;
#7834 = DIRECTION ( 'NONE',  ( -0.7313537016191756779, 0.6819983600624930364, -4.000536147326505450E-15 ) ) ;
#7835 = ORIENTED_EDGE ( 'NONE', *, *, #15896, .F. ) ;
#7836 =( GEOMETRIC_REPRESENTATION_CONTEXT ( 3 ) GLOBAL_UNCERTAINTY_ASSIGNED_CONTEXT ( ( #11207 ) ) GLOBAL_UNIT_ASSIGNED_CONTEXT ( ( #17292, #19413, #17774 ) ) REPRESENTATION_CONTEXT ( 'NONE', 'WORKASPACE' ) );
#7837 = CARTESIAN_POINT ( 'NONE',  ( 4.175572532730936537, -4.122058607836112110, 2.481766680540189602E-17 ) ) ;
#7838 = CARTESIAN_POINT ( 'NONE',  ( -42.54314575050785407, -4.000000000000034639, -7.500000000000007105 ) ) ;
#7839 = DIRECTION ( 'NONE',  ( 5.551115123125782702E-16, 1.201780285297635172E-31, -1.000000000000000000 ) ) ;
#7840 = DIRECTION ( 'NONE',  ( -1.066786462891689527E-26, -6.656013887802287108E-31, -1.000000000000000000 ) ) ;
#7841 = ADVANCED_FACE ( 'NONE', ( #12293 ), #19484, .T. ) ;
#7842 = CARTESIAN_POINT ( 'NONE',  ( 4.175326769692856210, 4.121399112977853996, -1.392133645916858894E-19 ) ) ;
#7843 = FACE_OUTER_BOUND ( 'NONE', #4680, .T. ) ;
#7844 = DIRECTION ( 'NONE',  ( -0.000000000000000000, 1.000000000000000000, -0.000000000000000000 ) ) ;
#7845 = CIRCLE ( 'NONE', #8995, 0.5000000000000017764 ) ;
#7846 = AXIS2_PLACEMENT_3D ( 'NONE', #9006, #19584, #21602 ) ;
#7847 = CARTESIAN_POINT ( 'NONE',  ( 8.954763739086851970, -1.500000000000001332, 6.678571428571422608 ) ) ;
#7848 = CARTESIAN_POINT ( 'NONE',  ( 37.34641016151398674, 0.3999999999999195310, -10.34641016151375581 ) ) ;
#7849 = EDGE_CURVE ( 'NONE', #19782, #273, #17613, .T. ) ;
#7850 =( LENGTH_UNIT ( ) NAMED_UNIT ( * ) SI_UNIT ( .MILLI., .METRE. ) );
#7851 = CARTESIAN_POINT ( 'NONE',  ( -6.938893903907228378E-14, 4.999999999999976907, -4.163336342344337027E-14 ) ) ;
#7852 = CARTESIAN_POINT ( 'NONE',  ( -1.170176016631815524E-15, 0.3423821193871265378, 3.499999999999994227 ) ) ;
#7853 = VERTEX_POINT ( 'NONE', #20298 ) ;
#7854 = MECHANICAL_DESIGN_GEOMETRIC_PRESENTATION_REPRESENTATION (  '', ( #12342 ), #2208 ) ;
#7855 = VERTEX_POINT ( 'NONE', #305 ) ;
#7856 = VERTEX_POINT ( 'NONE', #14529 ) ;
#7857 = ORIENTED_EDGE ( 'NONE', *, *, #6558, .F. ) ;
#7858 = FACE_BOUND ( 'NONE', #11465, .T. ) ;
#7859 = VECTOR ( 'NONE', #14192, 1000.000000000000000 ) ;
#7860 = CARTESIAN_POINT ( 'NONE',  ( 36.00000000029184832, 16.99999999900385461, -15.99999999999999289 ) ) ;
#7861 = ORIENTED_EDGE ( 'NONE', *, *, #21596, .F. ) ;
#7862 = FACE_OUTER_BOUND ( 'NONE', #8476, .T. ) ;
#7863 = DIRECTION ( 'NONE',  ( -1.000000000000000000, 4.440892098500654758E-16, 0.000000000000000000 ) ) ;
#7864 = DIRECTION ( 'NONE',  ( 0.000000000000000000, -1.000000000000000000, 0.000000000000000000 ) ) ;
#7865 = CARTESIAN_POINT ( 'NONE',  ( 66.26395429947837101, 0.000000000000000000, -5.999999999999908518 ) ) ;
#7866 = DIRECTION ( 'NONE',  ( 0.000000000000000000, -1.000000000000000000, 0.000000000000000000 ) ) ;
#7867 = CIRCLE ( 'NONE', #10501, 4.750000000000000000 ) ;
#7868 = DIRECTION ( 'NONE',  ( -3.885780586188016830E-16, -4.437342591868156373E-31, 1.000000000000000000 ) ) ;
#7869 = ADVANCED_FACE ( 'NONE', ( #5949 ), #2977, .T. ) ;
#7870 = DIRECTION ( 'NONE',  ( 1.000000000000000000, 4.440892098500626162E-16, 0.000000000000000000 ) ) ;
#7871 = CARTESIAN_POINT ( 'NONE',  ( 7.573440241539870499, -13.88616620752088160, 7.421600184846474768 ) ) ;
#7872 = CARTESIAN_POINT ( 'NONE',  ( 4.630153689607049650, -1.816756130622550821E-31, -5.371010071662842833 ) ) ;
#7873 = CARTESIAN_POINT ( 'NONE',  ( 2.775557561562891351E-14, 7.999999999999983125, -0.4999999999999865663 ) ) ;
#7874 = CARTESIAN_POINT ( 'NONE',  ( -12.84999999999999964, -2.000000000000001776, -2.550000000000000711 ) ) ;
#7875 = ADVANCED_FACE ( 'NONE', ( #16627 ), #9359, .T. ) ;
#7876 = CARTESIAN_POINT ( 'NONE',  ( 4.142654963991857286, 2.035398498734349193, -3.525413613457316409 ) ) ;
#7877 = EDGE_LOOP ( 'NONE', ( #13482, #18054, #21727, #13445 ) ) ;
#7878 = ITEM_DEFINED_TRANSFORMATION ( 'NONE', 'NONE', #19918,  #22115 ) ;
#7879 = CIRCLE ( 'NONE', #7515, 6.000000000000000000 ) ;
#7880 = VERTEX_POINT ( 'NONE', #13006 ) ;
#7881 = APPLICATION_CONTEXT ( 'automotive_design' ) ;
#7882 = AXIS2_PLACEMENT_3D ( 'NONE', #19418, #12354, #10483 ) ;
#7883 = ADVANCED_FACE ( 'NONE', ( #1936 ), #12349, .T. ) ;
#7885 = ORIENTED_EDGE ( 'NONE', *, *, #9831, .T. ) ;
#7884 = ORIENTED_EDGE ( 'NONE', *, *, #21708, .F. ) ;
#7886 = CYLINDRICAL_SURFACE ( 'NONE', #12156, 2.500000000000001332 ) ;
#7887 = PLANE ( 'NONE',  #15599 ) ;
#7888 = DIRECTION ( 'NONE',  ( -0.5000000000000014433, 0.8660254037844378194, -6.428855108704672838E-16 ) ) ;
#7889 = ORIENTED_EDGE ( 'NONE', *, *, #10538, .F. ) ;
#7890 = DIRECTION ( 'NONE',  ( 0.000000000000000000, -0.7453559924999247910, 0.6666666666666722918 ) ) ;
#7891 = CARTESIAN_POINT ( 'NONE',  ( 2.498001805406602216E-13, 2.500000000000002220, 6.000000000000158096 ) ) ;
#7892 = CARTESIAN_POINT ( 'NONE',  ( 4.175075985190096262, -2.060370777630097905, 3.568666869285575860 ) ) ;
#7893 = CARTESIAN_POINT ( 'NONE',  ( 0.000000000000000000, -0.5999999999999859890, 3.054668707061614086 ) ) ;
#7894 = CARTESIAN_POINT ( 'NONE',  ( -10.49999999999996803, -0.5000000000000004441, 9.250000000000035527 ) ) ;
#7895 = CARTESIAN_POINT ( 'NONE',  ( 78.36587326203827786, -2.990348597579628454, -5.999999999999998224 ) ) ;
#7896 = VECTOR ( 'NONE', #11067, 1000.000000000000000 ) ;
#7897 = DIRECTION ( 'NONE',  ( -1.000000000000000000, 4.190823558986610327E-31, -1.733449886265890494E-32 ) ) ;
#7898 = LINE ( 'NONE', #20140, #14369 ) ;
#7899 = PLANE ( 'NONE',  #20344 ) ;
#7900 = LINE ( 'NONE', #14954, #2793 ) ;
#7901 = DIRECTION ( 'NONE',  ( -0.5000000000000006661, 2.269329254444894332E-16, 0.8660254037844382635 ) ) ;
#7902 = CARTESIAN_POINT ( 'NONE',  ( 12.84999999999997300, -12.00000000000008704, -2.549999999999955413 ) ) ;
#7903 = CARTESIAN_POINT ( 'NONE',  ( 63.50658097017376491, -4.000000000000058620, -6.000000000000054179 ) ) ;
#7904 = ORIENTED_EDGE ( 'NONE', *, *, #21449, .F. ) ;
#7905 = DIRECTION ( 'NONE',  ( 0.6838270277705150724, -0.7296441571687829475, 1.226423327957133664E-16 ) ) ;
#7907 = ORIENTED_EDGE ( 'NONE', *, *, #20591, .T. ) ;
#7906 = ORIENTED_EDGE ( 'NONE', *, *, #1687, .F. ) ;
#7908 = UNCERTAINTY_MEASURE_WITH_UNIT (LENGTH_MEASURE( 1.000000000000000082E-05 ), #7850, 'distance_accuracy_value', 'NONE');
#7909 = ADVANCED_FACE ( 'NONE', ( #2174 ), #9362, .T. ) ;
#7910 = ORIENTED_EDGE ( 'NONE', *, *, #21335, .T. ) ;
#7912 = ORIENTED_EDGE ( 'NONE', *, *, #13472, .T. ) ;
#7911 = ORIENTED_EDGE ( 'NONE', *, *, #14558, .F. ) ;
#7913 = CIRCLE ( 'NONE', #791, 0.5000000000000002220 ) ;
#7914 = EDGE_LOOP ( 'NONE', ( #2438, #2152, #19133, #2554 ) ) ;
#7915 = CARTESIAN_POINT ( 'NONE',  ( 36.00000000029184832, -9.961476088449217059E-10, 0.000000000000000000 ) ) ;
#7916 = DIRECTION ( 'NONE',  ( -0.7071067811865485719, 0.7071067811865464625, 1.010793663541191362E-16 ) ) ;
#7917 = VERTEX_POINT ( 'NONE', #11335 ) ;
#7918 = FACE_OUTER_BOUND ( 'NONE', #2853, .T. ) ;
#7919 = ADVANCED_FACE ( 'NONE', ( #20068 ), #13871, .T. ) ;
#7920 = FACE_OUTER_BOUND ( 'NONE', #9644, .T. ) ;
#7921 = CARTESIAN_POINT ( 'NONE',  ( 37.86602540378461157, 10.49999999999999822, -6.500000000000005329 ) ) ;
#7922 = DIRECTION ( 'NONE',  ( 1.000000000000000000, 2.220446049250307657E-16, 0.000000000000000000 ) ) ;
#7923 = ADVANCED_FACE ( 'NONE', ( #198 ), #5609, .F. ) ;
#7924 = CARTESIAN_POINT ( 'NONE',  ( 24.75000000000000355, 2.000000000000029310, -3.469446951953614189E-15 ) ) ;
#7925 = CARTESIAN_POINT ( 'NONE',  ( 4.211399257449685685, -2.459727064652556194, -3.751161691472421733 ) ) ;
#7926 = LINE ( 'NONE', #13460, #23081 ) ;
#7927 = DIRECTION ( 'NONE',  ( -1.070367811204228886E-16, -0.8660254037844381525, -0.5000000000000009992 ) ) ;
#7928 = LINE ( 'NONE', #20646, #16428 ) ;
#7929 = CARTESIAN_POINT ( 'NONE',  ( 82.19834661797897013, -5.880524088665628923, 6.500000000000151879 ) ) ;
#7930 = AXIS2_PLACEMENT_3D ( 'NONE', #3955, #15956, #1619 ) ;
#7931 = MECHANICAL_DESIGN_GEOMETRIC_PRESENTATION_REPRESENTATION (  '', ( #16559 ), #4550 ) ;
#7932 = DIRECTION ( 'NONE',  ( -0.000000000000000000, -0.000000000000000000, 1.000000000000000000 ) ) ;
#7933 = CYLINDRICAL_SURFACE ( 'NONE', #14169, 3.999999999999994671 ) ;
#7934 = VERTEX_POINT ( 'NONE', #14761 ) ;
#7935 = UNCERTAINTY_MEASURE_WITH_UNIT (LENGTH_MEASURE( 1.000000000000000082E-05 ), #9094, 'distance_accuracy_value', 'NONE');
#7936 = ADVANCED_FACE ( 'NONE', ( #9469 ), #2057, .F. ) ;
#7938 = ORIENTED_EDGE ( 'NONE', *, *, #17433, .T. ) ;
#7937 = ORIENTED_EDGE ( 'NONE', *, *, #19146, .T. ) ;
#7939 = ADVANCED_FACE ( 'NONE', ( #20182 ), #4055, .F. ) ;
#7940 = VERTEX_POINT ( 'NONE', #11235 ) ;
#7941 = VERTEX_POINT ( 'NONE', #18411 ) ;
#7942 = VERTEX_POINT ( 'NONE', #7367 ) ;
#7943 = ORIENTED_EDGE ( 'NONE', *, *, #14431, .T. ) ;
#7944 = DIRECTION ( 'NONE',  ( 1.000000000000000000, -1.276756478318923119E-15, 1.342345546886807594E-15 ) ) ;
#7945 = ADVANCED_FACE ( 'NONE', ( #22061 ), #8598, .T. ) ;
#7946 = VECTOR ( 'NONE', #14807, 1000.000000000000000 ) ;
#7947 = AXIS2_PLACEMENT_3D ( 'NONE', #17055, #9659, #731 ) ;
#7948 = EDGE_CURVE ( 'NONE', #17189, #3914, #14246, .T. ) ;
#7949 = DIRECTION ( 'NONE',  ( -1.066786462891689527E-26, -6.656013887802287108E-31, -1.000000000000000000 ) ) ;
#7950 = ORIENTED_EDGE ( 'NONE', *, *, #22210, .F. ) ;
#7951 = CARTESIAN_POINT ( 'NONE',  ( 4.124214193018073793, -4.056676826581885997, 2.081674651455615798E-14 ) ) ;
#7952 = CARTESIAN_POINT ( 'NONE',  ( 37.43301270189239460, 0.2500000000000002220, -6.500000000000019540 ) ) ;
#7953 = DIRECTION ( 'NONE',  ( 0.000000000000000000, 0.000000000000000000, 1.000000000000000000 ) ) ;
#7954 = DIRECTION ( 'NONE',  ( -1.000000000000000000, 0.000000000000000000, 0.000000000000000000 ) ) ;
#7955 = CARTESIAN_POINT ( 'NONE',  ( -7.500000000000031974, -11.57130297831456645, 9.041853041249030554 ) ) ;
#7956 = DIRECTION ( 'NONE',  ( 4.190823558986625216E-31, -1.000000000000000000, 4.190823558986625216E-31 ) ) ;
#7957 = CARTESIAN_POINT ( 'NONE',  ( 7.949747468597695210, 47.94974746730969173, -29.00000000000000355 ) ) ;
#7958 = LINE ( 'NONE', #18904, #11140 ) ;
#7959 = EDGE_CURVE ( 'NONE', #9134, #3579, #14608, .T. ) ;
#7960 = EDGE_CURVE ( 'NONE', #5080, #8523, #8992, .T. ) ;
#7961 = ADVANCED_FACE ( 'NONE', ( #1895 ), #1558, .F. ) ;
#7962 = SURFACE_STYLE_USAGE ( .BOTH. , #683 ) ;
#7963 = CARTESIAN_POINT ( 'NONE',  ( -6.938893903907228378E-14, 0.7368602791855416445, -1.387778780781445676E-14 ) ) ;
#7964 = CARTESIAN_POINT ( 'NONE',  ( 30.60000000000000142, 2.775557561562891351E-14, -2.081668171172168513E-14 ) ) ;
#7965 = VECTOR ( 'NONE', #21273, 1000.000000000000114 ) ;
#7966 = ORIENTED_EDGE ( 'NONE', *, *, #13293, .T. ) ;
#7967 = ORIENTED_EDGE ( 'NONE', *, *, #4183, .T. ) ;
#7968 = EDGE_LOOP ( 'NONE', ( #13507, #406, #3713, #4034, #22538, #3323 ) ) ;
#7969 = EDGE_CURVE ( 'NONE', #20156, #17539, #9375, .T. ) ;
#7970 = PRODUCT_DEFINITION_SHAPE ( 'NONE', 'NONE',  #23286 ) ;
#7971 = ORIENTED_EDGE ( 'NONE', *, *, #14279, .F. ) ;
#7972 = CARTESIAN_POINT ( 'NONE',  ( -4.000000000000003553, 0.000000000000000000, -5.600000000000000533 ) ) ;
#7973 = CARTESIAN_POINT ( 'NONE',  ( 0.000000000000000000, 0.5000000000000108802, -10.86602540378443749 ) ) ;
#7974 = ORIENTED_EDGE ( 'NONE', *, *, #3079, .F. ) ;
#7975 = EDGE_CURVE ( 'NONE', #4281, #15019, #13505, .T. ) ;
#7976 = CIRCLE ( 'NONE', #8342, 2.500000000000001332 ) ;
#7977 = DIRECTION ( 'NONE',  ( -7.395570986446975166E-31, -3.382522293539642681E-32, -1.000000000000000000 ) ) ;
#7978 = DIRECTION ( 'NONE',  ( 0.000000000000000000, 0.000000000000000000, 1.000000000000000000 ) ) ;
#7979 = DIRECTION ( 'NONE',  ( 3.885780586188016830E-16, 4.437342591868156373E-31, -1.000000000000000000 ) ) ;
#7980 = CARTESIAN_POINT ( 'NONE',  ( -4.720100440590782931, 36.44386358679986415, -19.00000000000000355 ) ) ;
#7981 = VECTOR ( 'NONE', #17229, 1000.000000000000000 ) ;
#7982 = LINE ( 'NONE', #703, #10805 ) ;
#7983 = LINE ( 'NONE', #16674, #1548 ) ;
#7984 = CIRCLE ( 'NONE', #18125, 0.2500000000000002220 ) ;
#7985 = AXIS2_PLACEMENT_3D ( 'NONE', #13962, #12311, #9028 ) ;
#7986 = CARTESIAN_POINT ( 'NONE',  ( 2.789435349370705492E-14, 11.99999999999999645, -2.499999999999987121 ) ) ;
#7987 = AXIS2_PLACEMENT_3D ( 'NONE', #2038, #13955, #6674 ) ;
#7988 = DIRECTION ( 'NONE',  ( 0.000000000000000000, 0.000000000000000000, 1.000000000000000000 ) ) ;
#7989 = DIRECTION ( 'NONE',  ( 1.000000000000000000, 3.254448077276381206E-32, 1.066788928082016908E-26 ) ) ;
#7990 = DIRECTION ( 'NONE',  ( -2.220446049250313081E-16, 1.000000000000000000, -7.025792437124636392E-31 ) ) ;
#7991 = CARTESIAN_POINT ( 'NONE',  ( -2.060000000000002718, 2.522772406243550895E-16, -0.3080913168122707546 ) ) ;
#7992 = CYLINDRICAL_SURFACE ( 'NONE', #3249, 2.550000000000012701 ) ;
#7993 = COLOUR_RGB ( '', 0.08235294, 0.09019608, 0.10196078) ;
#7994 = CARTESIAN_POINT ( 'NONE',  ( 4.104070371397483541, 2.023683613428369110, -3.505122836902508698 ) ) ;
#7995 = ORIENTED_EDGE ( 'NONE', *, *, #18309, .T. ) ;
#7996 = CONTEXT_DEPENDENT_SHAPE_REPRESENTATION ( #13760, #10433 ) ;
#7997 = AXIS2_PLACEMENT_3D ( 'NONE', #15780, #16125, #12605 ) ;
#7998 = ORIENTED_EDGE ( 'NONE', *, *, #6222, .F. ) ;
#7999 = CIRCLE ( 'NONE', #13255, 2.499999999999993339 ) ;
#8000 = AXIS2_PLACEMENT_3D ( 'NONE', #15925, #1709, #15804 ) ;
#8001 = CIRCLE ( 'NONE', #15513, 6.500000000000052403 ) ;
#8003 = ORIENTED_EDGE ( 'NONE', *, *, #9187, .F. ) ;
#8002 = ORIENTED_EDGE ( 'NONE', *, *, #15948, .T. ) ;
#8004 = FACE_OUTER_BOUND ( 'NONE', #11605, .T. ) ;
#8005 = EDGE_CURVE ( 'NONE', #22532, #2832, #16489, .T. ) ;
#8006 = CARTESIAN_POINT ( 'NONE',  ( -6.938893903907228378E-14, -4.618802153517121312, -3.433295621305409107 ) ) ;
#8007 = CARTESIAN_POINT ( 'NONE',  ( 22.49999999999998224, 2.000000000000001776, -2.081668171172168513E-14 ) ) ;
#8008 = ORIENTED_EDGE ( 'NONE', *, *, #17314, .F. ) ;
#8009 = CARTESIAN_POINT ( 'NONE',  ( -4.580466231768955510, -0.7499999999999442668, -2.524719371073009810 ) ) ;
#8010 = DIRECTION ( 'NONE',  ( -0.9396926207859144231, 1.190256115088894218E-15, -0.3420201433256521706 ) ) ;
#8011 = CARTESIAN_POINT ( 'NONE',  ( -12.85000000000001386, -12.00000000000008704, -2.549999999999955413 ) ) ;
#8012 = CARTESIAN_POINT ( 'NONE',  ( -0.3461262719737096538, 4.658553426539353559, -3.671615880910378937 ) ) ;
#8013 = CARTESIAN_POINT ( 'NONE',  ( -3.200000000000119194, 1.999999999999911626, 7.500000000000062172 ) ) ;
#8014 = AXIS2_PLACEMENT_3D ( 'NONE', #10107, #9874, #4694 ) ;
#8015 = DIRECTION ( 'NONE',  ( 1.000000000000000000, 1.156482317317863245E-14, 0.000000000000000000 ) ) ;
#8016 = AXIS2_PLACEMENT_3D ( 'NONE', #8734, #6988, #14146 ) ;
#8017 = DIRECTION ( 'NONE',  ( 0.9961946980917454342, -4.598174816728386208E-16, -0.08715574274765928997 ) ) ;
#8018 = AXIS2_PLACEMENT_3D ( 'NONE', #3418, #14469, #21653 ) ;
#8019 = CONICAL_SURFACE ( 'NONE', #9902, 4.499999999999988454, 0.7853981633974396193 ) ;
#8020 = AXIS2_PLACEMENT_3D ( 'NONE', #2586, #4925, #13414 ) ;
#8021 = DIRECTION ( 'NONE',  ( 1.733449886265891589E-32, -4.190823558986610327E-31, 1.000000000000000000 ) ) ;
#8022 = DIRECTION ( 'NONE',  ( 0.000000000000000000, -0.000000000000000000, 1.000000000000000000 ) ) ;
#8023 = DIRECTION ( 'NONE',  ( -1.000000000000000000, -1.908195823574478022E-14, 2.087219286295281359E-14 ) ) ;
#8024 = VERTEX_POINT ( 'NONE', #10843 ) ;
#8025 = DIRECTION ( 'NONE',  ( -1.278478519402912229E-28, 1.110223024625156294E-16, 1.000000000000000000 ) ) ;
#8027 = ORIENTED_EDGE ( 'NONE', *, *, #1892, .F. ) ;
#8026 = ORIENTED_EDGE ( 'NONE', *, *, #3740, .T. ) ;
#8028 = ORIENTED_EDGE ( 'NONE', *, *, #950, .F. ) ;
#8029 = AXIS2_PLACEMENT_3D ( 'NONE', #9383, #3961, #7612 ) ;
#8031 = ORIENTED_EDGE ( 'NONE', *, *, #14291, .F. ) ;
#8030 = ORIENTED_EDGE ( 'NONE', *, *, #15423, .F. ) ;
#8032 = CONICAL_SURFACE ( 'NONE', #517, 4.000000000000000000, 1.047197551196595855 ) ;
#8033 = AXIS2_PLACEMENT_3D ( 'NONE', #17137, #13511, #937 ) ;
#8034 = CARTESIAN_POINT ( 'NONE',  ( -4.229990831856816236, -1.750000000000008882, 2.173440963673441750 ) ) ;
#8035 = AXIS2_PLACEMENT_3D ( 'NONE', #6790, #16177, #19252 ) ;
#8036 = CARTESIAN_POINT ( 'NONE',  ( 5.599999999999992539, 8.245366548881324970E-15, -2.500000000000001332 ) ) ;
#8037 = VECTOR ( 'NONE', #9424, 1000.000000000000000 ) ;
#8038 = EDGE_LOOP ( 'NONE', ( #21817, #11917 ) ) ;
#8039 = CARTESIAN_POINT ( 'NONE',  ( 66.26395429947839943, -7.000000000000006217, -6.499999999999999112 ) ) ;
#8040 = CARTESIAN_POINT ( 'NONE',  ( -12.85000000000001386, -12.00000000000006928, 4.163336342344337027E-14 ) ) ;
#8041 = DIRECTION ( 'NONE',  ( 0.000000000000000000, 0.000000000000000000, -1.000000000000000000 ) ) ;
#8042 = CARTESIAN_POINT ( 'NONE',  ( 3.344563996438205677, 2.687817229851463985, -0.1586754815284830145 ) ) ;
#8043 = DIRECTION ( 'NONE',  ( 2.013525853228518840E-32, -6.902532920683810383E-31, 1.000000000000000000 ) ) ;
#8044 = CARTESIAN_POINT ( 'NONE',  ( 7.602880770961811585, -2.006500808705091732, 8.461619612152045278 ) ) ;
#8045 = DIRECTION ( 'NONE',  ( -0.000000000000000000, -0.000000000000000000, 1.000000000000000000 ) ) ;
#8046 = EDGE_CURVE ( 'NONE', #6638, #17782, #8250, .T. ) ;
#8047 = CARTESIAN_POINT ( 'NONE',  ( 66.26395429947837101, -4.500000000000003553, 6.500000000000110134 ) ) ;
#8048 = AXIS2_PLACEMENT_3D ( 'NONE', #14948, #2478, #9433 ) ;
#8049 = FACE_OUTER_BOUND ( 'NONE', #740, .T. ) ;
#8050 = CARTESIAN_POINT ( 'NONE',  ( 1.110223024625156540E-13, 1.749999999999998002, -4.750000000000000888 ) ) ;
#8051 = CARTESIAN_POINT ( 'NONE',  ( -4.000000000000087041, 2.309401076758546445, -5.000000000000000888 ) ) ;
#8052 = AXIS2_PLACEMENT_3D ( 'NONE', #10974, #526, #14862 ) ;
#8053 = ORIENTED_EDGE ( 'NONE', *, *, #6079, .F. ) ;
#8054 = FILL_AREA_STYLE_COLOUR ( '', #3367 ) ;
#8056 = ORIENTED_EDGE ( 'NONE', *, *, #20454, .F. ) ;
#8055 = EDGE_LOOP ( 'NONE', ( #5696, #22004, #20597, #17603 ) ) ;
#8057 = ORIENTED_EDGE ( 'NONE', *, *, #13570, .F. ) ;
#8058 = ORIENTED_EDGE ( 'NONE', *, *, #2173, .T. ) ;
#8059 = ADVANCED_FACE ( 'NONE', ( #5561 ), #11609, .T. ) ;
#8060 = ORIENTED_EDGE ( 'NONE', *, *, #9103, .F. ) ;
#8061 = ORIENTED_EDGE ( 'NONE', *, *, #19283, .T. ) ;
#8062 = CARTESIAN_POINT ( 'NONE',  ( 4.175326769692857098, -2.060699556488887474, 3.569236330973490023 ) ) ;
#8063 = AXIS2_PLACEMENT_3D ( 'NONE', #11277, #18234, #5767 ) ;
#8064 = DIRECTION ( 'NONE',  ( 0.5833333333333320381, 1.429810390713075314E-30, -0.8122328620674146293 ) ) ;
#8065 = ORIENTED_EDGE ( 'NONE', *, *, #13250, .F. ) ;
#8066 = FACE_BOUND ( 'NONE', #5127, .T. ) ;
#8067 = EDGE_CURVE ( 'NONE', #6633, #3351, #12366, .T. ) ;
#8068 = DIRECTION ( 'NONE',  ( -1.066786462891689527E-26, -6.656013887802287108E-31, -1.000000000000000000 ) ) ;
#8069 = DIRECTION ( 'NONE',  ( 0.000000000000000000, 0.000000000000000000, -1.000000000000000000 ) ) ;
#8070 = DIRECTION ( 'NONE',  ( -0.2405376366294442736, -2.775557561562981331E-17, 0.9706398123736330597 ) ) ;
#8071 = CARTESIAN_POINT ( 'NONE',  ( 4.071447262713884463, 4.041451884327383226, 0.000000000000000000 ) ) ;
#8072 = EDGE_CURVE ( 'NONE', #10144, #14358, #15372, .T. ) ;
#8073 = DIRECTION ( 'NONE',  ( 2.242473278838646163E-61, 7.395570986447005381E-32, 1.000000000000000000 ) ) ;
#8074 = FACE_BOUND ( 'NONE', #4758, .T. ) ;
#8075 = DIRECTION ( 'NONE',  ( -7.860214984770699307E-18, 1.409037165336591006E-16, 1.000000000000000000 ) ) ;
#8076 = CARTESIAN_POINT ( 'NONE',  ( -55.05572809000130974, 1.387778780781445676E-14, -8.000000000000035527 ) ) ;
#8077 = VERTEX_POINT ( 'NONE', #6989 ) ;
#8078 = AXIS2_PLACEMENT_3D ( 'NONE', #8569, #21163, #5398 ) ;
#8079 = ADVANCED_FACE ( 'NONE', ( #12371 ), #19554, .T. ) ;
#8080 = SURFACE_STYLE_FILL_AREA ( #3020 ) ;
#8081 = CARTESIAN_POINT ( 'NONE',  ( 8.697224362267997222, -13.50000000000004974, 6.250000000000033751 ) ) ;
#8082 = CARTESIAN_POINT ( 'NONE',  ( -91.02295700146254376, -1.040834085586084257E-13, 6.338518968055040226 ) ) ;
#8083 = EDGE_CURVE ( 'NONE', #16003, #12006, #6372, .T. ) ;
#8084 = ORIENTED_EDGE ( 'NONE', *, *, #11976, .F. ) ;
#8085 = ORIENTED_EDGE ( 'NONE', *, *, #21191, .T. ) ;
#8086 = ORIENTED_EDGE ( 'NONE', *, *, #14460, .F. ) ;
#8087 = VERTEX_POINT ( 'NONE', #7737 ) ;
#8088 = DIRECTION ( 'NONE',  ( -1.000000000000000000, -1.479114197289397135E-31, -5.916456789157588541E-31 ) ) ;
#8089 = FACE_OUTER_BOUND ( 'NONE', #11365, .T. ) ;
#8090 = EDGE_LOOP ( 'NONE', ( #21326, #704, #17182, #22796 ) ) ;
#8091 = B_SPLINE_CURVE_WITH_KNOTS ( 'NONE', 3,
 ( #822, #15158, #4563, #8460 ),
 .UNSPECIFIED., .F., .F.,
 ( 4, 4 ),
 ( 2.309401076293742455E-07, 0.004330357959029834669 ),
 .UNSPECIFIED. ) ;
#8092 = DIRECTION ( 'NONE',  ( 1.000000000000000000, 4.252453317207022018E-31, -5.551115123125818447E-17 ) ) ;
#8093 = DIRECTION ( 'NONE',  ( -0.6819983600624981435, -0.7313537016191709039, 0.000000000000000000 ) ) ;
#8094 = EDGE_CURVE ( 'NONE', #13307, #20921, #4474, .T. ) ;
#8095 = CARTESIAN_POINT ( 'NONE',  ( 29.00000000029184832, 16.99999999900385461, -26.00000000000000000 ) ) ;
#8096 = EDGE_CURVE ( 'NONE', #3485, #7125, #449, .T. ) ;
#8097 = EDGE_CURVE ( 'NONE', #178, #10008, #14749, .T. ) ;
#8098 = VERTEX_POINT ( 'NONE', #11032 ) ;
#8099 = CIRCLE ( 'NONE', #3588, 0.5000000000000029976 ) ;
#8100 = CARTESIAN_POINT ( 'NONE',  ( -4.550510256924973795, 35.99999999900384751, -19.00000000000000000 ) ) ;
#8101 = DIRECTION ( 'NONE',  ( 1.733449886265891589E-32, -4.190823558986610327E-31, 1.000000000000000000 ) ) ;
#8102 = FACE_OUTER_BOUND ( 'NONE', #18673, .T. ) ;
#8103 = FACE_OUTER_BOUND ( 'NONE', #4571, .T. ) ;
#8104 = DIRECTION ( 'NONE',  ( -0.7071067811865485719, 0.7071067811865464625, 1.010793663541191485E-16 ) ) ;
#8105 = CONICAL_SURFACE ( 'NONE', #976, 4.750000000000000888, 1.047197551196600074 ) ;
#8106 = LINE ( 'NONE', #19157, #20812 ) ;
#8107 = CARTESIAN_POINT ( 'NONE',  ( 3.973110223767125859, 2.263145622885971846E-11, 3.565797985667392922 ) ) ;
#8108 = EDGE_CURVE ( 'NONE', #20416, #21919, #18099, .T. ) ;
#8109 = FACE_OUTER_BOUND ( 'NONE', #21413, .T. ) ;
#8110 = EDGE_CURVE ( 'NONE', #22558, #12086, #14676, .T. ) ;
#8111 = CARTESIAN_POINT ( 'NONE',  ( 2.500000000000005329, -3.183331332160763538E-15, 1.084202172485504434E-16 ) ) ;
#8112 = EDGE_CURVE ( 'NONE', #10141, #22558, #6124, .T. ) ;
#8113 = ITEM_DEFINED_TRANSFORMATION ( 'NONE', 'NONE', #10504,  #22115 ) ;
#8114 = EDGE_CURVE ( 'NONE', #19862, #10112, #1244, .T. ) ;
#8115 = ORIENTED_EDGE ( 'NONE', *, *, #21629, .F. ) ;
#8117 = ORIENTED_EDGE ( 'NONE', *, *, #3615, .T. ) ;
#8116 = ORIENTED_EDGE ( 'NONE', *, *, #21205, .F. ) ;
#8118 = AXIS2_PLACEMENT_3D ( 'NONE', #453, #9279, #13275 ) ;
#8119 = B_SPLINE_CURVE_WITH_KNOTS ( 'NONE', 3,
 ( #17201, #10266, #8504, #22745, #13912 ),
 .UNSPECIFIED., .F., .F.,
 ( 4, 1, 4 ),
 ( 0.000000000000000000, 0.002020725942163689639, 0.004041451884327379278 ),
 .UNSPECIFIED. ) ;
#8120 = DIRECTION ( 'NONE',  ( -2.168404344971008868E-16, 1.000000000000000000, -8.023096076392732812E-15 ) ) ;
#8121 = DIRECTION ( 'NONE',  ( 1.066786462891689527E-26, 6.656013887802287108E-31, 1.000000000000000000 ) ) ;
#8122 = AXIS2_PLACEMENT_3D ( 'NONE', #1062, #2690, #13639 ) ;
#8123 = DIRECTION ( 'NONE',  ( 0.000000000000000000, 0.000000000000000000, 1.000000000000000000 ) ) ;
#8124 = EDGE_LOOP ( 'NONE', ( #12653, #7314 ) ) ;
#8125 = DIRECTION ( 'NONE',  ( -0.000000000000000000, -0.000000000000000000, -1.000000000000000000 ) ) ;
#8126 = CARTESIAN_POINT ( 'NONE',  ( -47.82842712474651137, 4.371572875253824542, 7.500000000000020428 ) ) ;
#8127 = CARTESIAN_POINT ( 'NONE',  ( -0.9238745061264594938, 1.710161125106380631, 4.749999999999998224 ) ) ;
#8128 = DIRECTION ( 'NONE',  ( -3.254448077146059901E-32, -1.000000000000000000, -6.409494854920712161E-31 ) ) ;
#8129 = CARTESIAN_POINT ( 'NONE',  ( -42.54314575050792513, 3.999999999999996447, 16.42537846091821052 ) ) ;
#8130 = CIRCLE ( 'NONE', #11129, 4.249999999999965361 ) ;
#8131 = CARTESIAN_POINT ( 'NONE',  ( -3.066033393607966922E-14, 3.202582148906679471, 1.452965002680416617 ) ) ;
#8132 = CARTESIAN_POINT ( 'NONE',  ( 30.15500000000000114, 2.775557561562891351E-14, 2.499999999999981348 ) ) ;
#8133 = CARTESIAN_POINT ( 'NONE',  ( 0.000000000000000000, 0.000000000000000000, 3.469446951953614189E-15 ) ) ;
#8134 = ADVANCED_FACE ( 'NONE', ( #16323 ), #3122, .T. ) ;
#8135 = DIRECTION ( 'NONE',  ( -1.000000000000000000, 0.000000000000000000, -2.668805347656595124E-16 ) ) ;
#8136 = AXIS2_PLACEMENT_3D ( 'NONE', #8938, #19758, #3640 ) ;
#8137 = DIRECTION ( 'NONE',  ( -1.550910762415566494E-16, -1.000000000000000000, 8.135128085091684243E-31 ) ) ;
#8138 = CARTESIAN_POINT ( 'NONE',  ( -4.000000000000153655, -6.722053469410127491E-15, -3.142992957459292303 ) ) ;
#8139 = DIRECTION ( 'NONE',  ( -1.454462294001240516E-30, -1.000000000000000000, -0.000000000000000000 ) ) ;
#8140 = ADVANCED_FACE ( 'NONE', ( #14798 ), #5751, .T. ) ;
#8141 = ORIENTED_EDGE ( 'NONE', *, *, #14205, .F. ) ;
#8142 = VECTOR ( 'NONE', #14421, 1000.000000000000000 ) ;
#8144 = ORIENTED_EDGE ( 'NONE', *, *, #21222, .T. ) ;
#8143 = EDGE_LOOP ( 'NONE', ( #2668, #923, #19142, #4060 ) ) ;
#8145 = UNCERTAINTY_MEASURE_WITH_UNIT (LENGTH_MEASURE( 1.000000000000000082E-05 ), #10644, 'distance_accuracy_value', 'NONE');
#8146 = ORIENTED_EDGE ( 'NONE', *, *, #17174, .F. ) ;
#8148 = ORIENTED_EDGE ( 'NONE', *, *, #17919, .T. ) ;
#8147 = VERTEX_POINT ( 'NONE', #14563 ) ;
#8149 = ORIENTED_EDGE ( 'NONE', *, *, #8094, .T. ) ;
#8150 = CARTESIAN_POINT ( 'NONE',  ( 2.775557561562891351E-14, 11.99999999999999645, 6.938893903907228378E-15 ) ) ;
#8151 = VERTEX_POINT ( 'NONE', #22094 ) ;
#8152 = SURFACE_STYLE_FILL_AREA ( #17074 ) ;
#8153 = CARTESIAN_POINT ( 'NONE',  ( 4.158921614371303477, 1.986121848748768404, -3.559936047944503912 ) ) ;
#8154 = DIRECTION ( 'NONE',  ( 4.190823558986621713E-31, 1.000000000000000000, 4.190823558986611203E-31 ) ) ;
#8155 = CARTESIAN_POINT ( 'NONE',  ( -8.723547172042966480, -2.015988055643601395, 6.817515300137126921 ) ) ;
#8156 = CIRCLE ( 'NONE', #21317, 0.5000000000000019984 ) ;
#8157 = CARTESIAN_POINT ( 'NONE',  ( -95.20000000000052864, -2.700000000000119194, 1.000000000000000888 ) ) ;
#8158 = PRESENTATION_LAYER_ASSIGNMENT (  '', '', ( #5908 ) ) ;
#8159 = LINE ( 'NONE', #22626, #16246 ) ;
#8160 = FACE_OUTER_BOUND ( 'NONE', #5469, .T. ) ;
#8161 = CARTESIAN_POINT ( 'NONE',  ( 4.052432342741364657, 1.393590342654231984, 3.567979436357292755 ) ) ;
#8162 = VECTOR ( 'NONE', #4584, 1000.000000000000000 ) ;
#8163 = DIRECTION ( 'NONE',  ( -1.000000000000000000, -4.252453317207022018E-31, 5.551115123125818447E-17 ) ) ;
#8164 = CARTESIAN_POINT ( 'NONE',  ( 0.1388410611046090315, -2.351840044243034278, 2.926493552096019357 ) ) ;
#8165 = AXIS2_PLACEMENT_3D ( 'NONE', #18755, #14552, #8166 ) ;
#8166 = DIRECTION ( 'NONE',  ( 1.000000000000000000, 2.220446049250313081E-16, -3.656342123407104498E-48 ) ) ;
#8167 = DIRECTION ( 'NONE',  ( 0.7071067811865485719, -0.7071067811865464625, -1.010793663541191485E-16 ) ) ;
#8168 = CARTESIAN_POINT ( 'NONE',  ( 4.052416734886713279, -1.393505408945056478, -3.567979131523966174 ) ) ;
#8169 = PRODUCT ( 'hex flange bolt small_iso_ISO 4162 - M5 x 25 x 16-N', 'hex flange bolt small_iso_ISO 4162 - M5 x 25 x 16-N', '', ( #11285 ) ) ;
#8170 = ORIENTED_EDGE ( 'NONE', *, *, #16090, .F. ) ;
#8171 = PRESENTATION_STYLE_ASSIGNMENT (( #20995 ) ) ;
#8172 = CIRCLE ( 'NONE', #21333, 6.000000000000000000 ) ;
#8174 = VERTEX_POINT ( 'NONE', #12797 ) ;
#8173 = ORIENTED_EDGE ( 'NONE', *, *, #6360, .T. ) ;
#8175 = AXIS2_PLACEMENT_3D ( 'NONE', #2667, #9846, #5373 ) ;
#8176 = EDGE_LOOP ( 'NONE', ( #4726, #3825, #8872, #5847 ) ) ;
#8177 = ORIENTED_EDGE ( 'NONE', *, *, #22600, .F. ) ;
#8178 = AXIS2_PLACEMENT_3D ( 'NONE', #21991, #16672, #6226 ) ;
#8179 = ORIENTED_EDGE ( 'NONE', *, *, #23103, .T. ) ;
#8180 = EDGE_CURVE ( 'NONE', #2292, #4761, #18998, .T. ) ;
#8181 = ORIENTED_EDGE ( 'NONE', *, *, #11456, .F. ) ;
#8182 = CARTESIAN_POINT ( 'NONE',  ( 2.099999999999999645, 0.000000000000000000, -0.2800830152838856835 ) ) ;
#8183 = TOROIDAL_SURFACE ( 'NONE', #10060, 6.500000000000000888, 0.5000000000000000000 ) ;
#8184 = DIRECTION ( 'NONE',  ( 1.000000000000000000, 2.220446049250314067E-16, -5.825996348268307008E-33 ) ) ;
#8185 = EDGE_LOOP ( 'NONE', ( #3547, #18912, #18845, #20939, #23207, #1037, #9795, #22726 ) ) ;
#8186 = DIRECTION ( 'NONE',  ( -1.000000000000000000, 3.553773787591352645E-14, 0.000000000000000000 ) ) ;
#8187 = DIRECTION ( 'NONE',  ( 0.000000000000000000, 0.000000000000000000, 1.000000000000000000 ) ) ;
#8188 =( BOUNDED_SURFACE ( )  B_SPLINE_SURFACE ( 3, 2, ( 
 ( #6171, #15081, #11098 ),
 ( #9692, #4151, #11563 ),
 ( #760, #20168, #7580 ),
 ( #18400, #9347, #11323 ),
 ( #2159, #21942, #5832 ),
 ( #16735, #14978, #13687 ),
 ( #6280, #9927, #20752 ),
 ( #17077, #20870, #15204 ),
 ( #19090, #2981, #8280 ),
 ( #22861, #6738, #15436 ),
 ( #15555, #22743, #10152 ),
 ( #12017, #8394, #20979 ),
 ( #1112, #8155, #3098 ),
 ( #13455, #20639, #10037 ) ),
 .UNSPECIFIED., .F., .F., .F. ) 
 B_SPLINE_SURFACE_WITH_KNOTS ( ( 4, 2, 2, 2, 2, 2, 4 ),
 ( 3, 3 ),
 ( 0.000000000000000000, 0.0009656398008937970437, 0.001448459701340695620, 0.001931279601787594087, 0.002414099502234492555, 0.002896919402681391240, 0.003862559203575188175 ),
 ( 0.000000000000000000, 1.000000000000000000 ),
 .UNSPECIFIED. ) 
 GEOMETRIC_REPRESENTATION_ITEM ( )  RATIONAL_B_SPLINE_SURFACE ( (
 ( 1.000000000000000000, 0.7071067811865516806, 1.000000000000000000),
 ( 1.000000000000000000, 0.6907538105667505590, 1.000000000000000000),
 ( 1.000000000000000000, 0.6765417438349563550, 1.000000000000000000),
 ( 1.000000000000000000, 0.6623232117678578001, 1.000000000000000000),
 ( 1.000000000000000000, 0.6588386061807489646, 1.000000000000000000),
 ( 1.000000000000000000, 0.6547992448370589802, 1.000000000000000000),
 ( 1.000000000000000000, 0.6542040191408916572, 1.000000000000000000),
 ( 1.000000000000000000, 0.6557724471762208518, 1.000000000000000000),
 ( 1.000000000000000000, 0.6579729115736204781, 1.000000000000000000),
 ( 1.000000000000000000, 0.6644691908066192587, 1.000000000000000000),
 ( 1.000000000000000000, 0.6687559023949275483, 1.000000000000000000),
 ( 1.000000000000000000, 0.6835702420294330617, 1.000000000000000000),
 ( 1.000000000000000000, 0.6960226107070184298, 1.000000000000000000),
 ( 1.000000000000000000, 0.7071067811865491270, 1.000000000000000000) ) ) 
 REPRESENTATION_ITEM ( '' )  SURFACE ( )  );
#8189 = CARTESIAN_POINT ( 'NONE',  ( -8.326672684688674053E-14, -1.110223024625156540E-13, 7.500000000000000000 ) ) ;
#8190 = CARTESIAN_POINT ( 'NONE',  ( 3.000000000291852764, 42.99999999900385461, -19.00000000000000355 ) ) ;
#8191 = AXIS2_PLACEMENT_3D ( 'NONE', #4906, #3167, #1394 ) ;
#8192 = FACE_OUTER_BOUND ( 'NONE', #18564, .T. ) ;
#8193 = CARTESIAN_POINT ( 'NONE',  ( -7.500000000000034639, -11.35410196624970780, 9.250000000000056843 ) ) ;
#8194 = AXIS2_PLACEMENT_3D ( 'NONE', #3107, #1799, #21106 ) ;
#8195 = CARTESIAN_POINT ( 'NONE',  ( -4.000000000000095923, 0.3987449864459913784, -0.01220643443066572048 ) ) ;
#8196 = DIRECTION ( 'NONE',  ( 1.000000000000000000, 5.598259082250514647E-17, 3.330669073875432643E-16 ) ) ;
#8197 = DIRECTION ( 'NONE',  ( 2.891205793294678326E-16, 1.000000000000000000, -6.216092455583559018E-15 ) ) ;
#8198 = B_SPLINE_CURVE_WITH_KNOTS ( 'NONE', 3,
 ( #2094, #14681, #12805, #21867, #18104, #16092 ),
 .UNSPECIFIED., .F., .F.,
 ( 4, 2, 4 ),
 ( 0.000000000000000000, 0.002086519881787260184, 0.004173039763574520368 ),
 .UNSPECIFIED. ) ;
#8199 = CARTESIAN_POINT ( 'NONE',  ( 3.000000000291852764, 42.99999999900385461, -15.99999999999999289 ) ) ;
#8200 = VERTEX_POINT ( 'NONE', #12683 ) ;
#8201 = DIRECTION ( 'NONE',  ( -1.000000000000000000, 0.000000000000000000, 0.000000000000000000 ) ) ;
#8202 = AXIS2_PLACEMENT_3D ( 'NONE', #21879, #12939, #11169 ) ;
#8203 = LINE ( 'NONE', #19026, #11172 ) ;
#8204 = ORIENTED_EDGE ( 'NONE', *, *, #4200, .F. ) ;
#8205 = EDGE_CURVE ( 'NONE', #8955, #19419, #9394, .T. ) ;
#8206 = EDGE_LOOP ( 'NONE', ( #21980, #15169, #1877, #19698 ) ) ;
#8207 = EDGE_LOOP ( 'NONE', ( #22438, #2936, #18497, #22407 ) ) ;
#8208 = EDGE_LOOP ( 'NONE', ( #862, #633, #4193 ) ) ;
#8209 = MECHANICAL_DESIGN_GEOMETRIC_PRESENTATION_REPRESENTATION (  '', ( #1083 ), #8968 ) ;
#8210 = ADVANCED_FACE ( 'NONE', ( #2558 ), #6446, .T. ) ;
#8211 = CARTESIAN_POINT ( 'NONE',  ( 24.75000000000000355, 2.000000000000029310, -2.000000000000005329 ) ) ;
#8212 = CARTESIAN_POINT ( 'NONE',  ( 61.83096495907210510, -4.753799060524588782, 6.000000000000123457 ) ) ;
#8213 = ORIENTED_EDGE ( 'NONE', *, *, #6505, .T. ) ;
#8214 = CARTESIAN_POINT ( 'NONE',  ( -67.40537636629493079, 2.700000000000021938, 12.70639812373644517 ) ) ;
#8215 = CARTESIAN_POINT ( 'NONE',  ( 2.918498775983380256E-10, 2.999999999003851503, 0.000000000000000000 ) ) ;
#8216 = DIRECTION ( 'NONE',  ( -0.000000000000000000, -0.000000000000000000, 1.000000000000000000 ) ) ;
#8217 = ADVANCED_FACE ( 'NONE', ( #10090 ), #9494, .T. ) ;
#8218 = CARTESIAN_POINT ( 'NONE',  ( 22.49999999999996092, 2.000000000000043521, -17.75000000000001066 ) ) ;
#8219 = TOROIDAL_SURFACE ( 'NONE', #9670, 3.113037248396092416, 1.500000000000000000 ) ;
#8220 = DIRECTION ( 'NONE',  ( -1.000000000000000000, -6.224605580259554159E-31, 2.887593071917436153E-31 ) ) ;
#8221 = AXIS2_PLACEMENT_3D ( 'NONE', #13110, #19944, #16738 ) ;
#8222 = EDGE_CURVE ( 'NONE', #5689, #15196, #2443, .T. ) ;
#8223 = CARTESIAN_POINT ( 'NONE',  ( -7.176407415341960139, -0.3641807091869828650, 8.314790908397480251 ) ) ;
#8224 = EDGE_CURVE ( 'NONE', #6092, #17297, #7523, .T. ) ;
#8225 = CARTESIAN_POINT ( 'NONE',  ( 2.742413778650823364, 1.749999999999998002, -4.750000000000024869 ) ) ;
#8226 = DIRECTION ( 'NONE',  ( -0.000000000000000000, 1.000000000000000000, -0.000000000000000000 ) ) ;
#8227 = LINE ( 'NONE', #6584, #11766 ) ;
#8228 = DIRECTION ( 'NONE',  ( 0.1556420233463076119, 0.000000000000000000, 0.9878135252003121813 ) ) ;
#8229 = CARTESIAN_POINT ( 'NONE',  ( -2.000000000000020428, 3.464101615137764156, -3.142992957459267434 ) ) ;
#8230 = PRESENTATION_LAYER_ASSIGNMENT (  '', '', ( #22873 ) ) ;
#8231 = DIRECTION ( 'NONE',  ( 0.000000000000000000, -0.000000000000000000, 1.000000000000000000 ) ) ;
#8232 = EDGE_CURVE ( 'NONE', #3480, #7127, #3845, .T. ) ;
#8233 = AXIS2_PLACEMENT_3D ( 'NONE', #15938, #15710, #16052 ) ;
#8234 = EDGE_CURVE ( 'NONE', #10470, #4924, #13504, .T. ) ;
#8235 = CIRCLE ( 'NONE', #14248, 0.5000000000000029976 ) ;
#8236 = ORIENTED_EDGE ( 'NONE', *, *, #22926, .T. ) ;
#8237 = EDGE_CURVE ( 'NONE', #20666, #10858, #17129, .T. ) ;
#8239 = ORIENTED_EDGE ( 'NONE', *, *, #19460, .F. ) ;
#8238 = ORIENTED_EDGE ( 'NONE', *, *, #81, .T. ) ;
#8240 = PLANE ( 'NONE',  #6165 ) ;
#8241 = CARTESIAN_POINT ( 'NONE',  ( -56.54644007500109382, -1.110223024625156540E-13, -8.666666666666655416 ) ) ;
#8242 = DIRECTION ( 'NONE',  ( 0.000000000000000000, 1.000000000000000000, 0.000000000000000000 ) ) ;
#8244 = ORIENTED_EDGE ( 'NONE', *, *, #3392, .F. ) ;
#8243 = ADVANCED_FACE ( 'NONE', ( #18915 ), #2719, .T. ) ;
#8245 = LINE ( 'NONE', #8354, #13818 ) ;
#8246 = CARTESIAN_POINT ( 'NONE',  ( 4.071447262713891568, 4.041451884327377009, -2.081668171172168513E-14 ) ) ;
#8247 = EDGE_CURVE ( 'NONE', #14654, #12775, #15857, .T. ) ;
#8248 = CARTESIAN_POINT ( 'NONE',  ( 6.500000000000283329, 0.5000000000001669775, -5.999999999999943157 ) ) ;
#8249 = DIRECTION ( 'NONE',  ( 7.860214984770699307E-18, -1.409037165336591006E-16, -1.000000000000000000 ) ) ;
#8250 = CIRCLE ( 'NONE', #22525, 4.750000000000000888 ) ;
#8251 = CARTESIAN_POINT ( 'NONE',  ( 3.999999999999940936, 2.309401076758546445, -0.5000000000000004441 ) ) ;
#8252 = DIRECTION ( 'NONE',  ( 0.000000000000000000, -1.000000000000000000, 0.000000000000000000 ) ) ;
#8253 = CARTESIAN_POINT ( 'NONE',  ( -7.000000000000006217, -0.9711575687493188003, 9.522727272727280479 ) ) ;
#8254 = FACE_OUTER_BOUND ( 'NONE', #12034, .T. ) ;
#8255 = LINE ( 'NONE', #3199, #20190 ) ;
#8256 = CIRCLE ( 'NONE', #13877, 7.200000000000046363 ) ;
#8257 = CARTESIAN_POINT ( 'NONE',  ( 0.1217565302851317949, -3.710888496608955922, 0.5725525826504807014 ) ) ;
#8258 = ADVANCED_FACE ( 'NONE', ( #932 ), #8322, .T. ) ;
#8259 = CARTESIAN_POINT ( 'NONE',  ( -61.45000000000044338, 6.301625887772388776E-14, -1.999999999999973577 ) ) ;
#8260 = EDGE_CURVE ( 'NONE', #12892, #7709, #5379, .T. ) ;
#8261 = AXIS2_PLACEMENT_3D ( 'NONE', #4836, #12005, #8603 ) ;
#8262 = EDGE_LOOP ( 'NONE', ( #4952, #4607, #21324, #3917, #17788, #4249, #4394 ) ) ;
#8263 = EDGE_CURVE ( 'NONE', #15196, #7689, #6864, .T. ) ;
#8264 = DIRECTION ( 'NONE',  ( 0.6838270277705145173, -0.7296441571687835026, 8.100896937228356696E-17 ) ) ;
#8266 = ORIENTED_EDGE ( 'NONE', *, *, #5543, .T. ) ;
#8265 = ORIENTED_EDGE ( 'NONE', *, *, #20922, .T. ) ;
#8267 = ORIENTED_EDGE ( 'NONE', *, *, #15622, .F. ) ;
#8269 = ORIENTED_EDGE ( 'NONE', *, *, #9645, .F. ) ;
#8268 = EDGE_LOOP ( 'NONE', ( #2473, #18537, #4188, #9124 ) ) ;
#8270 = B_SPLINE_CURVE_WITH_KNOTS ( 'NONE', 3,
 ( #9049, #12216, #21539, #7070 ),
 .UNSPECIFIED., .F., .F.,
 ( 4, 4 ),
 ( 0.004330357959029895384, 0.008660484977952097319 ),
 .UNSPECIFIED. ) ;
#8271 = ORIENTED_EDGE ( 'NONE', *, *, #17717, .T. ) ;
#8272 = EDGE_CURVE ( 'NONE', #6061, #20542, #7480, .T. ) ;
#8273 = DIRECTION ( 'NONE',  ( 0.000000000000000000, 0.000000000000000000, -1.000000000000000000 ) ) ;
#8274 = CARTESIAN_POINT ( 'NONE',  ( -6.999999999999992006, -5.999999999999987566, 12.24999999999996980 ) ) ;
#8275 = DIRECTION ( 'NONE',  ( 0.000000000000000000, 0.000000000000000000, 1.000000000000000000 ) ) ;
#8276 = AXIS2_PLACEMENT_3D ( 'NONE', #1582, #14057, #4872 ) ;
#8277 = DIRECTION ( 'NONE',  ( -0.000000000000000000, -0.000000000000000000, 1.000000000000000000 ) ) ;
#8278 = B_SPLINE_CURVE_WITH_KNOTS ( 'NONE', 3,
 ( #21873, #8944, #462, #3537 ),
 .UNSPECIFIED., .F., .F.,
 ( 4, 4 ),
 ( 2.309401076647795080E-07, 0.004330357959029895384 ),
 .UNSPECIFIED. ) ;
#8279 = FACE_OUTER_BOUND ( 'NONE', #1701, .T. ) ;
#8280 = CARTESIAN_POINT ( 'NONE',  ( -7.551224464536099745, -2.121331013966575529, 7.234820221745193791 ) ) ;
#8281 = DIRECTION ( 'NONE',  ( 1.066788928082016908E-26, 3.471809175856251779E-58, -1.000000000000000000 ) ) ;
#8282 = CARTESIAN_POINT ( 'NONE',  ( 36.00000000029184832, 5.999999999003851059, -12.99999999999999822 ) ) ;
#8283 = CARTESIAN_POINT ( 'NONE',  ( 7.901093513163758075, -1.673173099260845120, 7.745538272134582236 ) ) ;
#8284 = CARTESIAN_POINT ( 'NONE',  ( 3.972058292797660872, 0.6948821373597369178, 3.565770528409109463 ) ) ;
#8285 = CARTESIAN_POINT ( 'NONE',  ( 0.000000000000000000, 0.000000000000000000, 0.000000000000000000 ) ) ;
#8286 = DIRECTION ( 'NONE',  ( 1.333893503340774882E-15, 2.778352770573747380E-17, 1.000000000000000000 ) ) ;
#8287 = CYLINDRICAL_SURFACE ( 'NONE', #20965, 6.999999999999999112 ) ;
#8288 = CARTESIAN_POINT ( 'NONE',  ( -6.000000000000088818, -5.300000000000027356, -8.000000000000007105 ) ) ;
#8289 = DIRECTION ( 'NONE',  ( 0.000000000000000000, -1.000000000000000000, 0.000000000000000000 ) ) ;
#8290 = ORIENTED_EDGE ( 'NONE', *, *, #4753, .T. ) ;
#8292 = ORIENTED_EDGE ( 'NONE', *, *, #15978, .T. ) ;
#8291 = ORIENTED_EDGE ( 'NONE', *, *, #8952, .F. ) ;
#8293 = VERTEX_POINT ( 'NONE', #22683 ) ;
#8294 = ADVANCED_FACE ( 'NONE', ( #9978 ), #6570, .F. ) ;
#8295 = ORIENTED_EDGE ( 'NONE', *, *, #12427, .F. ) ;
#8296 = ORIENTED_EDGE ( 'NONE', *, *, #679, .F. ) ;
#8297 = ADVANCED_FACE ( 'NONE', ( #7858, #20567, #4312 ), #4552, .T. ) ;
#8298 = EDGE_LOOP ( 'NONE', ( #4031, #1262, #19053, #4597, #7235, #15883, #12211 ) ) ;
#8299 = CARTESIAN_POINT ( 'NONE',  ( 4.132952817037863547, -2.031684012687259955, 3.518979934899753470 ) ) ;
#8300 = DIRECTION ( 'NONE',  ( 0.000000000000000000, 1.000000000000000000, 0.000000000000000000 ) ) ;
#8301 = VERTEX_POINT ( 'NONE', #10971 ) ;
#8302 = CARTESIAN_POINT ( 'NONE',  ( 3.999999999999940936, 2.309401076758546445, -0.5000000000000004441 ) ) ;
#8303 = ADVANCED_FACE ( 'NONE', ( #3389 ), #18168, .F. ) ;
#8304 = CARTESIAN_POINT ( 'NONE',  ( 1.199999999999992628, 0.6000000000000137446, 4.749999999999990230 ) ) ;
#8305 = DIRECTION ( 'NONE',  ( 2.013525853228507892E-32, 6.902532920683810383E-31, -1.000000000000000000 ) ) ;
#8306 = CARTESIAN_POINT ( 'NONE',  ( 54.42435809754109499, 0.000000000000000000, 6.500000000000144773 ) ) ;
#8307 = CIRCLE ( 'NONE', #6056, 2.549999999999996714 ) ;
#8308 = CARTESIAN_POINT ( 'NONE',  ( 86.00000000000137845, -13.52760560296348302, 6.500000000000117240 ) ) ;
#8309 = CARTESIAN_POINT ( 'NONE',  ( -1.387778780781445676E-14, -24.99999999999998224, 0.000000000000000000 ) ) ;
#8310 = CARTESIAN_POINT ( 'NONE',  ( 36.00000000029184832, 49.99999999900385461, -28.99999999999999645 ) ) ;
#8311 = FACE_OUTER_BOUND ( 'NONE', #13132, .T. ) ;
#8312 = CARTESIAN_POINT ( 'NONE',  ( 7.500000000000007105, -1.999999999999991340, 12.24999999999995559 ) ) ;
#8313 = ORIENTED_EDGE ( 'NONE', *, *, #15592, .F. ) ;
#8314 = CARTESIAN_POINT ( 'NONE',  ( -65.47859922179033276, 3.200000000000057021, -11.38422848940298593 ) ) ;
#8315 = CARTESIAN_POINT ( 'NONE',  ( 2.918498775983380256E-10, 2.999999999003851503, 0.000000000000000000 ) ) ;
#8316 = EDGE_LOOP ( 'NONE', ( #22539, #22030, #20274, #2584 ) ) ;
#8317 = VERTEX_POINT ( 'NONE', #23029 ) ;
#8318 = AXIS2_PLACEMENT_3D ( 'NONE', #5031, #22697, #11860 ) ;
#8319 = PRESENTATION_LAYER_ASSIGNMENT (  '', '', ( #16559 ) ) ;
#8320 = VERTEX_POINT ( 'NONE', #14630 ) ;
#8321 = EDGE_LOOP ( 'NONE', ( #15628, #3028, #12153 ) ) ;
#8322 = PLANE ( 'NONE',  #19640 ) ;
#8323 = DIRECTION ( 'NONE',  ( 1.000000000000000000, -4.190823558986621713E-31, 0.000000000000000000 ) ) ;
#8324 = ORIENTED_EDGE ( 'NONE', *, *, #6172, .F. ) ;
#8325 = B_SPLINE_CURVE_WITH_KNOTS ( 'NONE', 3,
 ( #7819, #14755, #16742, #22170, #20294, #18407 ),
 .UNSPECIFIED., .F., .F.,
 ( 4, 2, 4 ),
 ( 0.01103795673506161555, 0.01206113197427185514, 0.01308430721348209473 ),
 .UNSPECIFIED. ) ;
#8326 = DIRECTION ( 'NONE',  ( -0.9878135252003126254, -7.334277233329626759E-17, 0.1556420233463035041 ) ) ;
#8327 = CARTESIAN_POINT ( 'NONE',  ( 2.918498775983380256E-10, 2.999999999003851503, -45.00000000000000000 ) ) ;
#8328 = CARTESIAN_POINT ( 'NONE',  ( 0.2499999999999828748, 1.999999999999974021, -19.00000000000001066 ) ) ;
#8329 = DIRECTION ( 'NONE',  ( -1.066786462891689527E-26, -6.656013887802287108E-31, -1.000000000000000000 ) ) ;
#8330 = CARTESIAN_POINT ( 'NONE',  ( 116.5066492821803052, -7.708908342713760575, 6.000000000000102141 ) ) ;
#8331 = CARTESIAN_POINT ( 'NONE',  ( -7.490952241692738767, -0.6544882962156418627, 8.992386117842782411 ) ) ;
#8332 = DIRECTION ( 'NONE',  ( 3.032184104443272185E-30, 1.000000000000000000, -7.395570986447005381E-32 ) ) ;
#8333 = CARTESIAN_POINT ( 'NONE',  ( -4.690415759823443942, 0.7500000000000770495, -1.500000000000001332 ) ) ;
#8334 = AXIS2_PLACEMENT_3D ( 'NONE', #9608, #22423, #18655 ) ;
#8335 = AXIS2_PLACEMENT_3D ( 'NONE', #16665, #5986, #11149 ) ;
#8336 = LINE ( 'NONE', #22811, #9141 ) ;
#8337 = CARTESIAN_POINT ( 'NONE',  ( 4.050480423730733470, -1.376911654797405404, 3.567926555162027391 ) ) ;
#8338 = FACE_OUTER_BOUND ( 'NONE', #21444, .T. ) ;
#8339 = EDGE_CURVE ( 'NONE', #7626, #21891, #8372, .T. ) ;
#8340 = CARTESIAN_POINT ( 'NONE',  ( 12.84999999999997300, -12.00000000000006928, 4.163336342344337027E-14 ) ) ;
#8341 = ORIENTED_EDGE ( 'NONE', *, *, #6239, .F. ) ;
#8342 = AXIS2_PLACEMENT_3D ( 'NONE', #10043, #10269, #20875 ) ;
#8343 = ORIENTED_EDGE ( 'NONE', *, *, #4081, .T. ) ;
#8345 = ORIENTED_EDGE ( 'NONE', *, *, #16005, .F. ) ;
#8344 = ORIENTED_EDGE ( 'NONE', *, *, #11510, .F. ) ;
#8346 = AXIS2_PLACEMENT_3D ( 'NONE', #9482, #13485, #16985 ) ;
#8347 = DIRECTION ( 'NONE',  ( 1.000000000000000000, 0.000000000000000000, 0.000000000000000000 ) ) ;
#8348 = AXIS2_PLACEMENT_3D ( 'NONE', #7838, #9142, #4071 ) ;
#8349 =( NAMED_UNIT ( * ) SI_UNIT ( $, .STERADIAN. ) SOLID_ANGLE_UNIT ( ) );
#8350 = CARTESIAN_POINT ( 'NONE',  ( 82.19834661797897013, -5.880524088665628923, 6.500000000000151879 ) ) ;
#8351 = ORIENTED_EDGE ( 'NONE', *, *, #22186, .T. ) ;
#8352 = ADVANCED_BREP_SHAPE_REPRESENTATION ( '', ( #21131, #22115 ), #3350 ) ;
#8353 = CARTESIAN_POINT ( 'NONE',  ( -2.100000000000011635, 2.938364432290698513E-15, -5.000000000000003553 ) ) ;
#8354 = CARTESIAN_POINT ( 'NONE',  ( 118.0000000000018190, -4.000000000000003553, 6.000000000000109246 ) ) ;
#8355 = CARTESIAN_POINT ( 'NONE',  ( 6.495190528383217199, 0.000000000000000000, -3.750000000000000000 ) ) ;
#8356 = PRODUCT_DEFINITION_SHAPE ( 'NONE', 'NONE',  #3448 ) ;
#8357 = DIRECTION ( 'NONE',  ( -2.775557561562883647E-17, 3.406761633869147840E-16, -1.000000000000000000 ) ) ;
#8358 = EDGE_CURVE ( 'NONE', #3180, #5440, #18884, .T. ) ;
#8359 = CYLINDRICAL_SURFACE ( 'NONE', #17459, 0.8000000000000090372 ) ;
#8360 = AXIS2_PLACEMENT_3D ( 'NONE', #13316, #20499, #4351 ) ;
#8361 = DIRECTION ( 'NONE',  ( 1.000000000000000000, -5.551115122690166315E-17, -1.001543066815839268E-16 ) ) ;
#8362 = CARTESIAN_POINT ( 'NONE',  ( -65.55642023346354108, 0.5000000000000490719, -11.87813525200309783 ) ) ;
#8363 = CARTESIAN_POINT ( 'NONE',  ( -1.354447211139183087E-14, 6.219541108242056490E-16, 4.750000000000000000 ) ) ;
#8364 =( BOUNDED_CURVE ( )  B_SPLINE_CURVE ( 3, ( #1193, #17400, #6252, #11526 ),
 .UNSPECIFIED., .F., .T. ) 
 B_SPLINE_CURVE_WITH_KNOTS ( ( 4, 4 ),
 ( 3.665191429188050076, 4.712388980384689674 ),
 .UNSPECIFIED. ) 
 CURVE ( )  GEOMETRIC_REPRESENTATION_ITEM ( )  RATIONAL_B_SPLINE_CURVE ( ( 1.000000000000000000, 0.9106836025229521070, 0.9106836025229521070, 1.000000000000000000 ) ) 
 REPRESENTATION_ITEM ( '' )  );
#8365 = ADVANCED_FACE ( 'NONE', ( #8670 ), #7348, .T. ) ;
#8366 = CARTESIAN_POINT ( 'NONE',  ( -25.39999999999989555, 2.775557561562891351E-14, 6.938893903907228378E-14 ) ) ;
#8367 = VECTOR ( 'NONE', #3591, 1000.000000000000000 ) ;
#8368 = CARTESIAN_POINT ( 'NONE',  ( 4.175572532730925879, -4.122058607836116551, -1.269985433432320179E-15 ) ) ;
#8369 = AXIS2_PLACEMENT_3D ( 'NONE', #19143, #8092, #6219 ) ;
#8370 = AXIS2_PLACEMENT_3D ( 'NONE', #10983, #73, #9114 ) ;
#8371 = ORIENTED_EDGE ( 'NONE', *, *, #4342, .T. ) ;
#8372 = CIRCLE ( 'NONE', #17375, 4.500000000000031974 ) ;
#8373 = EDGE_CURVE ( 'NONE', #5891, #7803, #13634, .T. ) ;
#8374 = DIRECTION ( 'NONE',  ( -0.3780342595625901247, 0.9257916064627956798, 6.880178054722403855E-15 ) ) ;
#8375 = ADVANCED_FACE ( 'NONE', ( #9222 ), #16379, .T. ) ;
#8377 = EDGE_LOOP ( 'NONE', ( #6295, #11843, #1777, #8345, #11289 ) ) ;
#8376 = VERTEX_POINT ( 'NONE', #10436 ) ;
#8378 = UNCERTAINTY_MEASURE_WITH_UNIT (LENGTH_MEASURE( 1.000000000000000082E-05 ), #9637, 'distance_accuracy_value', 'NONE');
#8379 = VERTEX_POINT ( 'NONE', #15605 ) ;
#8381 = ORIENTED_EDGE ( 'NONE', *, *, #21075, .F. ) ;
#8380 = EDGE_LOOP ( 'NONE', ( #21504, #481, #16404, #2117 ) ) ;
#8382 = ORIENTED_EDGE ( 'NONE', *, *, #4338, .F. ) ;
#8383 = DIRECTION ( 'NONE',  ( -1.000000000000000000, 4.190823558986610327E-31, -1.733449886265890494E-32 ) ) ;
#8384 = DIRECTION ( 'NONE',  ( -1.000000000000000000, 4.615739097524200579E-16, 1.134196829589820086E-15 ) ) ;
#8385 = DIRECTION ( 'NONE',  ( 6.938893903907285176E-15, 1.000000000000000000, 2.736361264985384700E-30 ) ) ;
#8386 = AXIS2_PLACEMENT_3D ( 'NONE', #3133, #23136, #10299 ) ;
#8387 = VECTOR ( 'NONE', #10588, 1000.000000000000000 ) ;
#8388 = AXIS2_PLACEMENT_3D ( 'NONE', #18603, #13073, #608 ) ;
#8389 = DIRECTION ( 'NONE',  ( 0.000000000000000000, 0.000000000000000000, -1.000000000000000000 ) ) ;
#8390 = AXIS2_PLACEMENT_3D ( 'NONE', #9830, #22187, #15348 ) ;
#8391 = DIRECTION ( 'NONE',  ( 1.000000000000000000, 0.000000000000000000, 0.000000000000000000 ) ) ;
#8392 = AXIS2_PLACEMENT_3D ( 'NONE', #13343, #20523, #18857 ) ;
#8393 = EDGE_CURVE ( 'NONE', #3763, #4916, #11376, .T. ) ;
#8394 = CARTESIAN_POINT ( 'NONE',  ( -8.518530740350071184, -2.043531002858365309, 6.984205661426909906 ) ) ;
#8395 = AXIS2_PLACEMENT_3D ( 'NONE', #17906, #5443, #10836 ) ;
#8396 = CIRCLE ( 'NONE', #15895, 0.5000000000000038858 ) ;
#8397 = EDGE_CURVE ( 'NONE', #7880, #13843, #179, .T. ) ;
#8398 = EDGE_CURVE ( 'NONE', #6092, #2560, #4687, .T. ) ;
#8399 = CARTESIAN_POINT ( 'NONE',  ( 4.050880675075942072, -1.379097446046187558, -3.567934390854431204 ) ) ;
#8400 = DIRECTION ( 'NONE',  ( -2.220446049250313081E-16, 1.000000000000000000, -7.025792437124636392E-31 ) ) ;
#8401 = CARTESIAN_POINT ( 'NONE',  ( 24.75000000000001066, 2.000000000000099032, -17.49999999999998224 ) ) ;
#8402 = DIRECTION ( 'NONE',  ( 0.000000000000000000, 0.000000000000000000, -1.000000000000000000 ) ) ;
#8403 = CARTESIAN_POINT ( 'NONE',  ( 54.42435809754113052, -4.000000000000003553, -6.499999999999999112 ) ) ;
#8404 = DIRECTION ( 'NONE',  ( -1.066786462891689527E-26, -6.656013887802287108E-31, -1.000000000000000000 ) ) ;
#8405 = LINE ( 'NONE', #10046, #7426 ) ;
#8406 = DIRECTION ( 'NONE',  ( -1.000000000000000000, 0.000000000000000000, -4.336808689941968432E-16 ) ) ;
#8407 = ADVANCED_FACE ( 'NONE', ( #19372 ), #21536, .T. ) ;
#8408 = CARTESIAN_POINT ( 'NONE',  ( 3.948103430091018495, -2.682758828852505051, 2.353325403973639318 ) ) ;
#8409 = ORIENTED_EDGE ( 'NONE', *, *, #20226, .F. ) ;
#8410 = VECTOR ( 'NONE', #10561, 1000.000000000000000 ) ;
#8411 = EDGE_CURVE ( 'NONE', #20776, #11755, #13849, .T. ) ;
#8412 =( LENGTH_UNIT ( ) NAMED_UNIT ( * ) SI_UNIT ( .MILLI., .METRE. ) );
#8413 = AXIS2_PLACEMENT_3D ( 'NONE', #11165, #464, #7638 ) ;
#8415 = ORIENTED_EDGE ( 'NONE', *, *, #1485, .T. ) ;
#8414 = ORIENTED_EDGE ( 'NONE', *, *, #5967, .T. ) ;
#8416 = AXIS2_PLACEMENT_3D ( 'NONE', #7865, #18452, #4319 ) ;
#8417 = CIRCLE ( 'NONE', #6163, 4.000000000000023981 ) ;
#8418 = AXIS2_PLACEMENT_3D ( 'NONE', #4337, #12831, #720 ) ;
#8419 = ORIENTED_EDGE ( 'NONE', *, *, #12101, .T. ) ;
#8420 = ORIENTED_EDGE ( 'NONE', *, *, #10863, .T. ) ;
#8421 = ORIENTED_EDGE ( 'NONE', *, *, #13569, .F. ) ;
#8422 = DIRECTION ( 'NONE',  ( 3.885780586188016830E-16, 4.437342591868156373E-31, -1.000000000000000000 ) ) ;
#8423 = DIRECTION ( 'NONE',  ( -1.000000000000000000, -4.440892098500626162E-16, 5.551115123125782702E-16 ) ) ;
#8424 = ORIENTED_EDGE ( 'NONE', *, *, #10825, .F. ) ;
#8425 = LINE ( 'NONE', #22540, #13145 ) ;
#8426 = LINE ( 'NONE', #15584, #19633 ) ;
#8427 = AXIS2_PLACEMENT_3D ( 'NONE', #16819, #3815, #18189 ) ;
#8428 = DIRECTION ( 'NONE',  ( 3.885780586188016830E-16, 4.437342591868156373E-31, -1.000000000000000000 ) ) ;
#8429 = CYLINDRICAL_SURFACE ( 'NONE', #19465, 2.099999999999999645 ) ;
#8430 = DIRECTION ( 'NONE',  ( 0.6819983600624998088, -0.7313537016191693496, 0.000000000000000000 ) ) ;
#8431 = CIRCLE ( 'NONE', #14817, 0.4999999999999987232 ) ;
#8432 = CARTESIAN_POINT ( 'NONE',  ( -6.961281259571849844, 35.99999999900387593, -26.48045177140990702 ) ) ;
#8433 = CYLINDRICAL_SURFACE ( 'NONE', #18826, 2.499999999999993783 ) ;
#8434 = CARTESIAN_POINT ( 'NONE',  ( 63.50658097017375070, -4.000000000000003553, 6.000000000000185629 ) ) ;
#8435 = DIRECTION ( 'NONE',  ( -1.000000000000000000, 0.000000000000000000, 0.000000000000000000 ) ) ;
#8436 = EDGE_CURVE ( 'NONE', #6938, #20539, #12119, .T. ) ;
#8437 = LINE ( 'NONE', #18660, #12252 ) ;
#8438 = VERTEX_POINT ( 'NONE', #21270 ) ;
#8439 = CARTESIAN_POINT ( 'NONE',  ( 4.175813232069149450, -2.061359961916378492, -3.570380186727402538 ) ) ;
#8440 = DIRECTION ( 'NONE',  ( 0.000000000000000000, -1.000000000000000000, 0.000000000000000000 ) ) ;
#8441 = ORIENTED_EDGE ( 'NONE', *, *, #14485, .T. ) ;
#8442 = EDGE_CURVE ( 'NONE', #7710, #14484, #1606, .T. ) ;
#8443 = CIRCLE ( 'NONE', #11804, 0.5000000000000004441 ) ;
#8444 = ORIENTED_EDGE ( 'NONE', *, *, #7304, .T. ) ;
#8445 = AXIS2_PLACEMENT_3D ( 'NONE', #4233, #22017, #2131 ) ;
#8446 = ORIENTED_EDGE ( 'NONE', *, *, #7270, .F. ) ;
#8447 = PRESENTATION_LAYER_ASSIGNMENT (  '', '', ( #191 ) ) ;
#8448 = CARTESIAN_POINT ( 'NONE',  ( 4.175813232069142344, 2.061359961916371830, 3.570380186727395433 ) ) ;
#8449 = CARTESIAN_POINT ( 'NONE',  ( -0.6543461111163908495, -4.241015250120827140, -0.1391502195351569937 ) ) ;
#8450 = EDGE_LOOP ( 'NONE', ( #18392, #13560, #5888, #15770 ) ) ;
#8451 = FACE_OUTER_BOUND ( 'NONE', #7795, .T. ) ;
#8452 = CARTESIAN_POINT ( 'NONE',  ( -12.85000000000005649, -12.00000000000011191, -6.249999999999936051 ) ) ;
#8453 = CARTESIAN_POINT ( 'NONE',  ( -25.39999999999989910, 2.775557561562891351E-14, 2.500000000000059952 ) ) ;
#8454 = DIRECTION ( 'NONE',  ( 1.000000000000000000, 1.479114197289397135E-31, 5.916456789157588541E-31 ) ) ;
#8455 = CARTESIAN_POINT ( 'NONE',  ( -7.000000000000020428, -0.9711575687493234632, 9.522727272727296466 ) ) ;
#8456 = CARTESIAN_POINT ( 'NONE',  ( 42.00000000000017764, 5.500000000000001776, 2.000000000000057288 ) ) ;
#8457 = AXIS2_PLACEMENT_3D ( 'NONE', #128, #5065, #21194 ) ;
#8458 = CARTESIAN_POINT ( 'NONE',  ( -3.499999999708153453, 38.99999999900385461, -18.50000000000000355 ) ) ;
#8459 = AXIS2_PLACEMENT_3D ( 'NONE', #12238, #1781, #14367 ) ;
#8460 = CARTESIAN_POINT ( 'NONE',  ( -6.495190528383335327, 5.000000000000018652, -3.750000000000003553 ) ) ;
#8461 = CARTESIAN_POINT ( 'NONE',  ( 4.175813232069142344, -2.061359961916364725, 3.570380186727402538 ) ) ;
#8462 = CARTESIAN_POINT ( 'NONE',  ( -42.54314575050795355, 3.999999999999996447, -7.500000000000007105 ) ) ;
#8463 = DIRECTION ( 'NONE',  ( 1.000000000000000000, -3.739292825994448183E-14, 0.000000000000000000 ) ) ;
#8464 = VERTEX_POINT ( 'NONE', #864 ) ;
#8465 = ADVANCED_FACE ( 'NONE', ( #12863 ), #22035, .F. ) ;
#8466 = ORIENTED_EDGE ( 'NONE', *, *, #9090, .T. ) ;
#8467 = CARTESIAN_POINT ( 'NONE',  ( 12.49999999999995914, 2.775557561562891351E-14, -9.500000000000003553 ) ) ;
#8468 = CIRCLE ( 'NONE', #8842, 0.5000000000000028866 ) ;
#8470 = ORIENTED_EDGE ( 'NONE', *, *, #13317, .T. ) ;
#8469 = VERTEX_POINT ( 'NONE', #7693 ) ;
#8471 = VECTOR ( 'NONE', #15976, 1000.000000000000000 ) ;
#8472 = DIRECTION ( 'NONE',  ( -1.000000000000000000, 1.550910762415526064E-16, 0.000000000000000000 ) ) ;
#8473 = DIRECTION ( 'NONE',  ( 0.000000000000000000, 0.000000000000000000, -1.000000000000000000 ) ) ;
#8474 = EDGE_CURVE ( 'NONE', #17683, #955, #9453, .T. ) ;
#8475 = DIRECTION ( 'NONE',  ( -0.7313537016191730133, 0.6819983600624958120, -5.924440990721418971E-17 ) ) ;
#8476 = EDGE_LOOP ( 'NONE', ( #8181, #17579, #15971, #17534 ) ) ;
#8477 = DIRECTION ( 'NONE',  ( -1.000000000000000000, -2.699383410053119644E-30, -3.330669073875432643E-16 ) ) ;
#8478 = DIRECTION ( 'NONE',  ( 1.000000000000000000, 3.254448077276381206E-32, 1.066788928082016908E-26 ) ) ;
#8479 = CARTESIAN_POINT ( 'NONE',  ( 12.84999999999995879, -0.5000000000000004441, 6.250000000000047073 ) ) ;
#8480 = DIRECTION ( 'NONE',  ( 0.000000000000000000, 0.000000000000000000, 1.000000000000000000 ) ) ;
#8481 = CARTESIAN_POINT ( 'NONE',  ( 2.682243648011605863, 3.070208061305347957, -0.04852650426600601391 ) ) ;
#8482 = CONICAL_SURFACE ( 'NONE', #7361, 7.500000000000001776, 1.308996938995750092 ) ;
#8483 = CARTESIAN_POINT ( 'NONE',  ( -3.345653888883665772, 2.687187980154696731, -5.460849780464863024 ) ) ;
#8484 = DIRECTION ( 'NONE',  ( -1.000000000000000000, -2.168404344971017743E-16, 1.780660105995169760E-30 ) ) ;
#8485 = DIRECTION ( 'NONE',  ( 3.885780586188016830E-16, 4.437342591868156373E-31, -1.000000000000000000 ) ) ;
#8486 = DIRECTION ( 'NONE',  ( -0.000000000000000000, -0.000000000000000000, 1.000000000000000000 ) ) ;
#8487 = CARTESIAN_POINT ( 'NONE',  ( 4.104070371397483541, -4.047367226856738220, 0.000000000000000000 ) ) ;
#8488 = ORIENTED_EDGE ( 'NONE', *, *, #21771, .T. ) ;
#8489 = VECTOR ( 'NONE', #11901, 1000.000000000000000 ) ;
#8490 =( LENGTH_UNIT ( ) NAMED_UNIT ( * ) SI_UNIT ( .MILLI., .METRE. ) );
#8492 = EDGE_LOOP ( 'NONE', ( #11983, #20151, #12055 ) ) ;
#8491 = ORIENTED_EDGE ( 'NONE', *, *, #8498, .F. ) ;
#8493 = VECTOR ( 'NONE', #9996, 1000.000000000000000 ) ;
#8495 = ORIENTED_EDGE ( 'NONE', *, *, #1118, .T. ) ;
#8494 = ORIENTED_EDGE ( 'NONE', *, *, #18015, .T. ) ;
#8496 = CARTESIAN_POINT ( 'NONE',  ( -9.714451465470119729E-14, -2.775557561562891351E-14, -7.500000000000062172 ) ) ;
#8497 = DIRECTION ( 'NONE',  ( -0.6666666666666649643, -4.683861624749726065E-31, -0.7453559924999314523 ) ) ;
#8498 = EDGE_CURVE ( 'NONE', #6, #12162, #14479, .T. ) ;
#8499 = DIRECTION ( 'NONE',  ( 2.013525853228507892E-32, 6.902532920683810383E-31, -1.000000000000000000 ) ) ;
#8500 = AXIS2_PLACEMENT_3D ( 'NONE', #5122, #12283, #12048 ) ;
#8501 = CARTESIAN_POINT ( 'NONE',  ( 4.154306624731114006, 2.398490048084875426, -3.721999068284411738 ) ) ;
#8502 = CARTESIAN_POINT ( 'NONE',  ( 2.775557561562891351E-14, 2.999999999999999112, -12.50000000000001066 ) ) ;
#8503 = DIRECTION ( 'NONE',  ( 0.000000000000000000, 0.000000000000000000, 1.000000000000000000 ) ) ;
#8504 = CARTESIAN_POINT ( 'NONE',  ( 3.806834918298641401, 2.168404344971008868E-16, 3.499999999999994227 ) ) ;
#8505 = EDGE_CURVE ( 'NONE', #21059, #6039, #4971, .T. ) ;
#8506 = PLANE ( 'NONE',  #17388 ) ;
#8507 = EDGE_CURVE ( 'NONE', #9447, #15190, #6042, .T. ) ;
#8508 = CARTESIAN_POINT ( 'NONE',  ( 4.180231680468788902, -2.085385483809538254, 3.570466434508600351 ) ) ;
#8509 = DIRECTION ( 'NONE',  ( 0.000000000000000000, 1.000000000000000000, 0.000000000000000000 ) ) ;
#8510 = ADVANCED_FACE ( 'NONE', ( #13334 ), #480, .T. ) ;
#8511 = AXIS2_PLACEMENT_3D ( 'NONE', #17706, #15704, #3140 ) ;
#8512 = DIRECTION ( 'NONE',  ( 1.454462294001240516E-30, 1.000000000000000000, 0.000000000000000000 ) ) ;
#8513 = CARTESIAN_POINT ( 'NONE',  ( 29.00000000029184832, 16.99999999900385461, -26.00000000000000000 ) ) ;
#8514 = CARTESIAN_POINT ( 'NONE',  ( -4.000000000000103029, 2.471528634177575512, -3.686887442155210692 ) ) ;
#8515 = DIRECTION ( 'NONE',  ( 1.000000000000000000, 1.910522504832140594E-31, -5.551115123125818447E-17 ) ) ;
#8516 = ORIENTED_EDGE ( 'NONE', *, *, #17784, .F. ) ;
#8518 = ORIENTED_EDGE ( 'NONE', *, *, #5746, .F. ) ;
#8517 = VERTEX_POINT ( 'NONE', #4143 ) ;
#8519 = ORIENTED_EDGE ( 'NONE', *, *, #16903, .F. ) ;
#8520 = EDGE_CURVE ( 'NONE', #7692, #22215, #17291, .T. ) ;
#8521 = EDGE_CURVE ( 'NONE', #1669, #19695, #3489, .T. ) ;
#8522 = VECTOR ( 'NONE', #8563, 1000.000000000000000 ) ;
#8523 = VERTEX_POINT ( 'NONE', #13096 ) ;
#8524 = ORIENTED_EDGE ( 'NONE', *, *, #10798, .F. ) ;
#8525 = VECTOR ( 'NONE', #16024, 1000.000000000000000 ) ;
#8526 = ORIENTED_EDGE ( 'NONE', *, *, #22790, .T. ) ;
#8527 = CARTESIAN_POINT ( 'NONE',  ( 4.163336342344337027E-14, 3.469446951953614189E-14, -3.000000000000002665 ) ) ;
#8528 = CARTESIAN_POINT ( 'NONE',  ( 119.5756419024616690, -7.000000000000062172, -6.500000000000033751 ) ) ;
#8529 = EDGE_CURVE ( 'NONE', #13843, #5583, #21816, .T. ) ;
#8530 = ORIENTED_EDGE ( 'NONE', *, *, #50, .T. ) ;
#8531 = DIRECTION ( 'NONE',  ( 2.013525853228507892E-32, 6.902532920683810383E-31, -1.000000000000000000 ) ) ;
#8532 = EDGE_CURVE ( 'NONE', #15636, #6497, #21932, .T. ) ;
#8533 = CARTESIAN_POINT ( 'NONE',  ( 2.000000000000029310, 3.464101615137740175, -5.600000000000000533 ) ) ;
#8534 = ADVANCED_FACE ( 'NONE', ( #20160 ), #403, .F. ) ;
#8535 = CARTESIAN_POINT ( 'NONE',  ( 84.32438398889958364, -11.28140466348809312, -6.500000000000026645 ) ) ;
#8536 = LINE ( 'NONE', #4559, #20814 ) ;
#8537 = DIRECTION ( 'NONE',  ( 0.000000000000000000, 0.000000000000000000, 1.000000000000000000 ) ) ;
#8538 = CARTESIAN_POINT ( 'NONE',  ( -4.330127018922255822, -9.714451465470119729E-14, 7.499999999999985789 ) ) ;
#8539 = EDGE_CURVE ( 'NONE', #10463, #3117, #13648, .T. ) ;
#8540 = DIRECTION ( 'NONE',  ( 5.551115123125677932E-17, 0.000000000000000000, -1.000000000000000000 ) ) ;
#8541 = LINE ( 'NONE', #916, #9361 ) ;
#8542 = CARTESIAN_POINT ( 'NONE',  ( -6.839530184912448796, 13.99859551563898563, -18.01161035304105695 ) ) ;
#8543 = AXIS2_PLACEMENT_3D ( 'NONE', #4208, #708, #22225 ) ;
#8544 = CARTESIAN_POINT ( 'NONE',  ( -7.500000000000008882, -2.439868446130576629, 9.052558787159767917 ) ) ;
#8545 = AXIS2_PLACEMENT_3D ( 'NONE', #10904, #16194, #12324 ) ;
#8546 = ORIENTED_EDGE ( 'NONE', *, *, #6354, .T. ) ;
#8547 =( NAMED_UNIT ( * ) SI_UNIT ( $, .STERADIAN. ) SOLID_ANGLE_UNIT ( ) );
#8548 = DIRECTION ( 'NONE',  ( -9.121204216617949000E-31, -1.000000000000000000, 6.982962677686261977E-15 ) ) ;
#8549 = LINE ( 'NONE', #19486, #8564 ) ;
#8551 = ORIENTED_EDGE ( 'NONE', *, *, #779, .F. ) ;
#8550 = EDGE_LOOP ( 'NONE', ( #14631, #21558, #605, #7427 ) ) ;
#8552 = AXIS2_PLACEMENT_3D ( 'NONE', #5569, #14383, #12380 ) ;
#8553 = ADVANCED_FACE ( 'NONE', ( #4032 ), #14768, .T. ) ;
#8554 = ORIENTED_EDGE ( 'NONE', *, *, #17222, .T. ) ;
#8555 = ORIENTED_EDGE ( 'NONE', *, *, #8659, .T. ) ;
#8556 = PRODUCT_DEFINITION_SHAPE ( 'NONE', 'NONE',  #23274 ) ;
#8557 = EDGE_LOOP ( 'NONE', ( #9104, #18246, #7034, #12126 ) ) ;
#8558 = CARTESIAN_POINT ( 'NONE',  ( -6.938893903907228378E-14, -4.618802153517121312, -5.000000000000011546 ) ) ;
#8559 = DIRECTION ( 'NONE',  ( 1.000000000000000000, 2.699383410053119644E-30, 3.330669073875432643E-16 ) ) ;
#8560 = AXIS2_PLACEMENT_3D ( 'NONE', #12197, #6691, #19264 ) ;
#8561 = CARTESIAN_POINT ( 'NONE',  ( -50.65685424949267457, -7.200000000000049916, 8.000000000000035527 ) ) ;
#8562 = EDGE_CURVE ( 'NONE', #4606, #3634, #3143, .T. ) ;
#8563 = DIRECTION ( 'NONE',  ( 1.000000000000000000, 5.598259082250514647E-17, 3.330669073875432643E-16 ) ) ;
#8564 = VECTOR ( 'NONE', #15712, 1000.000000000000114 ) ;
#8565 = DIRECTION ( 'NONE',  ( 1.134196829589822059E-15, 6.741645191078037727E-32, -1.000000000000000000 ) ) ;
#8566 = FACE_OUTER_BOUND ( 'NONE', #4489, .T. ) ;
#8567 = CIRCLE ( 'NONE', #8935, 4.000000000000045297 ) ;
#8568 = CARTESIAN_POINT ( 'NONE',  ( -7.920269128372646072, -0.6322607639407478164, 7.713069291591470034 ) ) ;
#8569 = CARTESIAN_POINT ( 'NONE',  ( 0.000000000000000000, -1.750000000000001554, 0.000000000000000000 ) ) ;
#8570 = CARTESIAN_POINT ( 'NONE',  ( 6.000000000291855429, -9.961476088449217059E-10, 0.000000000000000000 ) ) ;
#8571 = CARTESIAN_POINT ( 'NONE',  ( 0.000000000000000000, 0.000000000000000000, 3.469446951953614189E-15 ) ) ;
#8572 = DIRECTION ( 'NONE',  ( 0.000000000000000000, 0.000000000000000000, 1.000000000000000000 ) ) ;
#8574 = VECTOR ( 'NONE', #23111, 1000.000000000000000 ) ;
#8573 = DIRECTION ( 'NONE',  ( -7.216449660063526979E-15, -6.938893903907237055E-15, -1.000000000000000000 ) ) ;
#8575 = CARTESIAN_POINT ( 'NONE',  ( 4.330127018922095949, 4.689110867544643568, -7.500000000000003553 ) ) ;
#8576 = EDGE_LOOP ( 'NONE', ( #21181, #15483, #15541, #18702 ) ) ;
#8577 = ORIENTED_EDGE ( 'NONE', *, *, #11696, .T. ) ;
#8578 = CARTESIAN_POINT ( 'NONE',  ( 5.550000000291854363, 42.99999999900385461, -19.00000000000000355 ) ) ;
#8579 = AXIS2_PLACEMENT_3D ( 'NONE', #4303, #18552, #20323 ) ;
#8581 = ORIENTED_EDGE ( 'NONE', *, *, #14821, .F. ) ;
#8580 = VERTEX_POINT ( 'NONE', #16602 ) ;
#8582 = AXIS2_PLACEMENT_3D ( 'NONE', #3870, #11393, #7756 ) ;
#8583 = CIRCLE ( 'NONE', #21001, 0.4999999999999990563 ) ;
#8584 = CARTESIAN_POINT ( 'NONE',  ( -0.1404048886733319235, -4.699864953788127409, -3.686887068327057371 ) ) ;
#8585 = EDGE_CURVE ( 'NONE', #6752, #8151, #750, .T. ) ;
#8586 = VERTEX_POINT ( 'NONE', #2854 ) ;
#8587 = CARTESIAN_POINT ( 'NONE',  ( 0.000000000000000000, 0.000000000000000000, -4.974599999999998801 ) ) ;
#8588 = ORIENTED_EDGE ( 'NONE', *, *, #17555, .F. ) ;
#8589 = DIRECTION ( 'NONE',  ( 1.733449886265891589E-32, -4.190823558986610327E-31, 1.000000000000000000 ) ) ;
#8590 = CARTESIAN_POINT ( 'NONE',  ( 3.997250504095358981, -1.750000000000003331, 2.576559036326539154 ) ) ;
#8591 = CARTESIAN_POINT ( 'NONE',  ( -65.55642023346344160, -2.700000000000091216, -11.87813525200317954 ) ) ;
#8592 = ADVANCED_FACE ( 'NONE', ( #19199 ), #19658, .T. ) ;
#8593 = CARTESIAN_POINT ( 'NONE',  ( 3.951447005078446484, -1.347150628109143877, 3.500000000000002220 ) ) ;
#8594 = DIRECTION ( 'NONE',  ( 0.8660254037844385966, 0.000000000000000000, -0.5000000000000001110 ) ) ;
#8595 = DIRECTION ( 'NONE',  ( -0.7313537016191756779, 0.6819983600624930364, 2.105690488111832645E-15 ) ) ;
#8596 = DIRECTION ( 'NONE',  ( 1.000000000000000000, -1.847414967615758933E-47, 3.885780586188017323E-16 ) ) ;
#8597 = PRESENTATION_STYLE_ASSIGNMENT (( #17526 ) ) ;
#8598 = TOROIDAL_SURFACE ( 'NONE', #1107, 2.500000000000002220, 0.5000000000000000000 ) ;
#8599 = DIRECTION ( 'NONE',  ( 2.220446049250314067E-16, -1.000000000000000000, 7.025792437124636392E-31 ) ) ;
#8600 = SHAPE_REPRESENTATION_RELATIONSHIP ( 'NONE' , 'NONE' ,  #10586, #18435 ) ;
#8601 = VERTEX_POINT ( 'NONE', #17306 ) ;
#8602 = ADVANCED_FACE ( 'NONE', ( #10031 ), #13448, .F. ) ;
#8603 = DIRECTION ( 'NONE',  ( -0.9476909587615098829, 0.3191893586598564259, -2.220446049250313081E-16 ) ) ;
#8605 = EDGE_LOOP ( 'NONE', ( #22530, #7317, #12616, #15108 ) ) ;
#8604 = ORIENTED_EDGE ( 'NONE', *, *, #18330, .T. ) ;
#8606 = PRESENTATION_LAYER_ASSIGNMENT (  '', '', ( #11604 ) ) ;
#8607 = ORIENTED_EDGE ( 'NONE', *, *, #1810, .F. ) ;
#8609 = ORIENTED_EDGE ( 'NONE', *, *, #12894, .T. ) ;
#8608 = EDGE_LOOP ( 'NONE', ( #7347, #7069, #19366, #22965 ) ) ;
#8610 = DIRECTION ( 'NONE',  ( -1.550910762415566494E-16, -1.000000000000000000, 8.135128085091684243E-31 ) ) ;
#8611 = FACE_OUTER_BOUND ( 'NONE', #21752, .T. ) ;
#8612 = DIRECTION ( 'NONE',  ( 0.000000000000000000, -1.000000000000000000, 0.000000000000000000 ) ) ;
#8613 = AXIS2_PLACEMENT_3D ( 'NONE', #419, #3941, #7591 ) ;
#8614 = FACE_OUTER_BOUND ( 'NONE', #21580, .T. ) ;
#8615 = CIRCLE ( 'NONE', #1482, 0.4999999999999994449 ) ;
#8616 = LINE ( 'NONE', #6851, #3965 ) ;
#8617 = DIRECTION ( 'NONE',  ( -0.9878135252003127365, 1.532010627492774434E-16, 0.1556420233463029767 ) ) ;
#8618 = CARTESIAN_POINT ( 'NONE',  ( 8.502135871254308697, -13.49242826152325314, 6.995667647939222356 ) ) ;
#8619 = DIRECTION ( 'NONE',  ( -1.000000000000000000, 0.000000000000000000, 0.000000000000000000 ) ) ;
#8620 = CARTESIAN_POINT ( 'NONE',  ( -47.47487373415325607, 4.018019484660559471, 7.500000000000007105 ) ) ;
#8621 = CONICAL_SURFACE ( 'NONE', #14635, 2.500000000000015543, 0.9599310885968873608 ) ;
#8622 = CARTESIAN_POINT ( 'NONE',  ( -3.679171394226111058, -2.494631558665882931, -0.3503314178413123314 ) ) ;
#8623 = CARTESIAN_POINT ( 'NONE',  ( 4.229990831856820677, -1.750000000000000222, -2.173440963673463067 ) ) ;
#8624 = PRODUCT_DEFINITION ( 'UNKNOWN', '', #13895, #13584 ) ;
#8625 = DIRECTION ( 'NONE',  ( 1.000000000000000000, -4.190823558986621713E-31, 0.000000000000000000 ) ) ;
#8626 = CARTESIAN_POINT ( 'NONE',  ( -7.500000000000007105, -11.35410196624970780, 9.250000000000035527 ) ) ;
#8627 = CARTESIAN_POINT ( 'NONE',  ( -4.000000000000108358, -2.512220745329347693, -3.469390707569752763 ) ) ;
#8628 = DIRECTION ( 'NONE',  ( 1.000000000000000000, 0.000000000000000000, 0.000000000000000000 ) ) ;
#8629 = ORIENTED_EDGE ( 'NONE', *, *, #20925, .F. ) ;
#8630 = EDGE_CURVE ( 'NONE', #21672, #13557, #14763, .T. ) ;
#8631 =( NAMED_UNIT ( * ) PLANE_ANGLE_UNIT ( ) SI_UNIT ( $, .RADIAN. ) );
#8633 = ORIENTED_EDGE ( 'NONE', *, *, #14775, .T. ) ;
#8632 = ORIENTED_EDGE ( 'NONE', *, *, #17731, .T. ) ;
#8634 = ORIENTED_EDGE ( 'NONE', *, *, #21078, .T. ) ;
#8635 = EDGE_CURVE ( 'NONE', #22909, #17679, #22738, .T. ) ;
#8636 = EDGE_LOOP ( 'NONE', ( #10185, #11818, #19779, #20770 ) ) ;
#8637 = VECTOR ( 'NONE', #7810, 1000.000000000000000 ) ;
#8638 = APPLICATION_CONTEXT ( 'automotive_design' ) ;
#8639 = ORIENTED_EDGE ( 'NONE', *, *, #21320, .T. ) ;
#8640 = EDGE_CURVE ( 'NONE', #20161, #23027, #18847, .T. ) ;
#8641 = VERTEX_POINT ( 'NONE', #22855 ) ;
#8642 = DIRECTION ( 'NONE',  ( -0.000000000000000000, -0.000000000000000000, 1.000000000000000000 ) ) ;
#8643 = CARTESIAN_POINT ( 'NONE',  ( 1.387778780781445676E-14, 4.618802153517020059, -5.600000000000000533 ) ) ;
#8644 = ORIENTED_EDGE ( 'NONE', *, *, #6485, .F. ) ;
#8645 = DIRECTION ( 'NONE',  ( 1.550910762415566494E-16, 1.000000000000000000, -8.135128085091684243E-31 ) ) ;
#8646 = CARTESIAN_POINT ( 'NONE',  ( 4.175813232069142344, 2.061359961916364725, -3.570380186727397209 ) ) ;
#8647 = CARTESIAN_POINT ( 'NONE',  ( 36.00000000029184832, 16.99999999900385461, -19.49999999999998934 ) ) ;
#8648 = FACE_OUTER_BOUND ( 'NONE', #3233, .T. ) ;
#8649 = CARTESIAN_POINT ( 'NONE',  ( 0.000000000000000000, 0.000000000000000000, 0.000000000000000000 ) ) ;
#8650 = DIRECTION ( 'NONE',  ( 4.844685039213900252E-16, 1.201780285297635172E-31, -1.000000000000000000 ) ) ;
#8651 = FACE_OUTER_BOUND ( 'NONE', #5700, .T. ) ;
#8652 = EDGE_CURVE ( 'NONE', #5256, #17475, #504, .T. ) ;
#8653 = CARTESIAN_POINT ( 'NONE',  ( 5.600000000000000533, 2.020725942163695166, -3.500000000000034195 ) ) ;
#8654 = DIRECTION ( 'NONE',  ( 1.000000000000000000, 2.312964634635752325E-16, -1.880120159248731926E-30 ) ) ;
#8655 = TOROIDAL_SURFACE ( 'NONE', #16162, 6.500000000000000888, 0.5000000000000000000 ) ;
#8656 = FACE_OUTER_BOUND ( 'NONE', #22234, .T. ) ;
#8657 = CARTESIAN_POINT ( 'NONE',  ( 63.50658097017376491, -6.500000000000061284, -6.000000000000054179 ) ) ;
#8658 = VERTEX_POINT ( 'NONE', #13680 ) ;
#8659 = EDGE_CURVE ( 'NONE', #8098, #17679, #19277, .T. ) ;
#8660 = FILL_AREA_STYLE ('',( #3482 ) ) ;
#8661 = DIRECTION ( 'NONE',  ( 0.000000000000000000, 1.000000000000000000, 0.000000000000000000 ) ) ;
#8662 = PLANE ( 'NONE',  #22467 ) ;
#8664 = ORIENTED_EDGE ( 'NONE', *, *, #13029, .T. ) ;
#8663 = ORIENTED_EDGE ( 'NONE', *, *, #4306, .F. ) ;
#8665 = B_SPLINE_CURVE_WITH_KNOTS ( 'NONE', 3,
 ( #14088, #3396, #3723, #5621 ),
 .UNSPECIFIED., .F., .F.,
 ( 4, 4 ),
 ( 0.000000000000000000, 0.002080789711329242460 ),
 .UNSPECIFIED. ) ;
#8666 = EDGE_CURVE ( 'NONE', #20884, #10194, #7278, .T. ) ;
#8667 = ORIENTED_EDGE ( 'NONE', *, *, #21500, .F. ) ;
#8668 = EDGE_CURVE ( 'NONE', #14653, #19191, #6273, .T. ) ;
#8669 = ORIENTED_EDGE ( 'NONE', *, *, #2635, .T. ) ;
#8670 = FACE_OUTER_BOUND ( 'NONE', #16868, .T. ) ;
#8671 = DIRECTION ( 'NONE',  ( 0.7071067811865490160, 0.7071067811865460184, 1.565905175853766674E-16 ) ) ;
#8672 = AXIS2_PLACEMENT_3D ( 'NONE', #9409, #11163, #19989 ) ;
#8673 = CARTESIAN_POINT ( 'NONE',  ( 8.954763739086823549, -0.5000000000000004441, 6.678571428571450141 ) ) ;
#8674 = CARTESIAN_POINT ( 'NONE',  ( 0.000000000000000000, -1.750000000000025757, 4.749999999999973355 ) ) ;
#8675 = CARTESIAN_POINT ( 'NONE',  ( 0.000000000000000000, -14.99999999999997513, -1.387778780781445676E-14 ) ) ;
#8676 = CARTESIAN_POINT ( 'NONE',  ( -42.54314575050796776, 5.299999999999991829, -8.000000000000035527 ) ) ;
#8677 = DIRECTION ( 'NONE',  ( -0.000000000000000000, -0.000000000000000000, 1.000000000000000000 ) ) ;
#8678 = B_SPLINE_CURVE_WITH_KNOTS ( 'NONE', 3,
 ( #17645, #6963, #12704, #16100, #19409, #12586, #1872, #21546, #3312, #10477, #5429, #19772, #16215, #3652, #10819, #130 ),
 .UNSPECIFIED., .F., .F.,
 ( 4, 3, 3, 3, 3, 4 ),
 ( -2.111273352579345034E-06, 4.235164736271501695E-22, 3.519286887791630951E-05, 7.191842652066397345E-05, 0.0001049868727093587593, 0.0001382836236822092074 ),
 .UNSPECIFIED. ) ;
#8679 = CARTESIAN_POINT ( 'NONE',  ( -8.148407558029997944, -0.5601289046717349285, 7.382406087064004474 ) ) ;
#8680 = CARTESIAN_POINT ( 'NONE',  ( -1.393927851585492039, 4.043713361053525190, -3.526374918436834704 ) ) ;
#8681 = ADVANCED_FACE ( 'NONE', ( #15548 ), #14013, .T. ) ;
#8682 = EDGE_CURVE ( 'NONE', #6499, #18441, #18674, .T. ) ;
#8683 = DIRECTION ( 'NONE',  ( -1.000000000000000000, -1.424116703980846297E-16, 1.095779650622964657E-32 ) ) ;
#8684 = ADVANCED_FACE ( 'NONE', ( #4608 ), #20973, .T. ) ;
#8685 = FACE_OUTER_BOUND ( 'NONE', #11057, .T. ) ;
#8686 = CARTESIAN_POINT ( 'NONE',  ( 42.00000000000020606, 2.999999999999999112, -15.50000000000004086 ) ) ;
#8687 = DIRECTION ( 'NONE',  ( 0.000000000000000000, 0.000000000000000000, -1.000000000000000000 ) ) ;
#8688 = CARTESIAN_POINT ( 'NONE',  ( -3.436319922986721842, 2.634841920957935901, -3.531542292955571316 ) ) ;
#8689 = DIRECTION ( 'NONE',  ( 1.000000000000000000, 2.168404344971017743E-16, -1.780660105995169760E-30 ) ) ;
#8691 = AXIS2_PLACEMENT_3D ( 'NONE', #2075, #10785, #23162 ) ;
#8690 = DIRECTION ( 'NONE',  ( 1.000000000000000000, -4.437342591868175641E-31, 3.330669073875457788E-16 ) ) ;
#8692 = VECTOR ( 'NONE', #21258, 1000.000000000000000 ) ;
#8693 = ORIENTED_EDGE ( 'NONE', *, *, #22114, .F. ) ;
#8694 = ADVANCED_FACE ( 'NONE', ( #12012 ), #17779, .T. ) ;
#8695 = EDGE_CURVE ( 'NONE', #18640, #14890, #17426, .T. ) ;
#8696 = ORIENTED_EDGE ( 'NONE', *, *, #14993, .T. ) ;
#8697 = CARTESIAN_POINT ( 'NONE',  ( -12.84999999999999964, -2.000000000000001776, 0.000000000000000000 ) ) ;
#8699 = ORIENTED_EDGE ( 'NONE', *, *, #19579, .F. ) ;
#8698 = ORIENTED_EDGE ( 'NONE', *, *, #3989, .F. ) ;
#8700 = DIRECTION ( 'NONE',  ( -1.000000000000000000, -1.479114197289397135E-31, -5.916456789157588541E-31 ) ) ;
#8701 = DIRECTION ( 'NONE',  ( 2.775557561562883955E-17, -3.406761633869148826E-16, 1.000000000000000000 ) ) ;
#8702 = LINE ( 'NONE', #12214, #15748 ) ;
#8703 = ORIENTED_EDGE ( 'NONE', *, *, #3516, .F. ) ;
#8704 = CARTESIAN_POINT ( 'NONE',  ( 27.94974746859769255, 27.94974746730969528, -26.50000000000000000 ) ) ;
#8705 = AXIS2_PLACEMENT_3D ( 'NONE', #19472, #497, #16361 ) ;
#8706 = AXIS2_PLACEMENT_3D ( 'NONE', #15776, #18227, #2095 ) ;
#8707 = CARTESIAN_POINT ( 'NONE',  ( 0.8691381963085855755, 0.6000000000000128564, -4.444516329276114064 ) ) ;
#8708 = CYLINDRICAL_SURFACE ( 'NONE', #18816, 0.5000000000000004441 ) ;
#8709 = LINE ( 'NONE', #21306, #6527 ) ;
#8710 = DIRECTION ( 'NONE',  ( 0.7071067811865532349, -0.7071067811865416886, -1.565905175853764455E-16 ) ) ;
#8711 = FACE_OUTER_BOUND ( 'NONE', #21782, .T. ) ;
#8712 = CARTESIAN_POINT ( 'NONE',  ( 4.158921614371306141, -1.986121848748789498, 3.559936047944491477 ) ) ;
#8713 = CARTESIAN_POINT ( 'NONE',  ( -12.84999999999999964, -2.000000000000001776, 2.549999999999997158 ) ) ;
#8714 = CARTESIAN_POINT ( 'NONE',  ( 10.50000000000000888, -2.000000000000001776, 5.750000000000005329 ) ) ;
#8715 = ADVANCED_FACE ( 'NONE', ( #15656 ), #2370, .T. ) ;
#8716 = ORIENTED_EDGE ( 'NONE', *, *, #14877, .F. ) ;
#8717 = DIRECTION ( 'NONE',  ( -6.459415335821039936E-12, -9.062299871385531922E-12, 1.000000000000000000 ) ) ;
#8718 = CIRCLE ( 'NONE', #16962, 4.500000000000031974 ) ;
#8719 = AXIS2_PLACEMENT_3D ( 'NONE', #1389, #3161, #4793 ) ;
#8721 = ORIENTED_EDGE ( 'NONE', *, *, #15256, .F. ) ;
#8720 = ORIENTED_EDGE ( 'NONE', *, *, #16417, .T. ) ;
#8722 = VECTOR ( 'NONE', #6617, 1000.000000000000000 ) ;
#8723 = EDGE_CURVE ( 'NONE', #10112, #4169, #22673, .T. ) ;
#8724 = EDGE_LOOP ( 'NONE', ( #14166, #11868, #114, #16485 ) ) ;
#8726 = EDGE_LOOP ( 'NONE', ( #9679, #17563, #19228, #19810 ) ) ;
#8725 = ORIENTED_EDGE ( 'NONE', *, *, #12220, .T. ) ;
#8727 = CARTESIAN_POINT ( 'NONE',  ( 6.500000000000227374, 2.500000000000141220, 4.163336342344337027E-14 ) ) ;
#8728 = CARTESIAN_POINT ( 'NONE',  ( 77.42435809754135789, -6.499999999999811706, 6.500000000000137668 ) ) ;
#8729 = CARTESIAN_POINT ( 'NONE',  ( -50.65685424949267457, -7.200000000000071232, -8.000000000000007105 ) ) ;
#8730 = DIRECTION ( 'NONE',  ( 5.551115123125818447E-17, 6.982962677686276177E-15, 1.000000000000000000 ) ) ;
#8731 = AXIS2_PLACEMENT_3D ( 'NONE', #3447, #48, #2021 ) ;
#8732 = CARTESIAN_POINT ( 'NONE',  ( 5.213674118230995802, 0.7500000000000492939, -3.000000000000002665 ) ) ;
#8733 = DIRECTION ( 'NONE',  ( -1.000000000000000000, -2.699383410053119644E-30, -3.330669073875432643E-16 ) ) ;
#8734 = CARTESIAN_POINT ( 'NONE',  ( 124.5000000000019469, -7.000000000000062172, 2.081668171172168513E-14 ) ) ;
#8735 = DIRECTION ( 'NONE',  ( 5.551115123125677932E-17, 0.000000000000000000, -1.000000000000000000 ) ) ;
#8736 = FACE_OUTER_BOUND ( 'NONE', #19310, .T. ) ;
#8737 = FACE_OUTER_BOUND ( 'NONE', #19519, .T. ) ;
#8738 = AXIS2_PLACEMENT_3D ( 'NONE', #16041, #12516, #7014 ) ;
#8739 = DIRECTION ( 'NONE',  ( 0.000000000000000000, 0.000000000000000000, -1.000000000000000000 ) ) ;
#8740 = CARTESIAN_POINT ( 'NONE',  ( -8.954763739086851970, -0.5000000000000004441, 6.678571428571422608 ) ) ;
#8741 = CIRCLE ( 'NONE', #3104, 1.749999999999999778 ) ;
#8742 = AXIS2_PLACEMENT_3D ( 'NONE', #5826, #2275, #9573 ) ;
#8743 = DIRECTION ( 'NONE',  ( -4.190823558986625216E-31, 1.000000000000000000, -4.190823558986625216E-31 ) ) ;
#8744 = CARTESIAN_POINT ( 'NONE',  ( 12.49999999999992362, 1.250000000000015099, -9.500000000000001776 ) ) ;
#8745 = DIRECTION ( 'NONE',  ( 1.000000000000000000, 0.000000000000000000, 0.000000000000000000 ) ) ;
#8746 = DIRECTION ( 'NONE',  ( 3.885780586188016830E-16, 4.437342591868156373E-31, -1.000000000000000000 ) ) ;
#8747 = PRODUCT_DEFINITION_SHAPE ( 'NONE', 'NONE',  #23282 ) ;
#8748 = EDGE_LOOP ( 'NONE', ( #10855, #17151 ) ) ;
#8750 = ORIENTED_EDGE ( 'NONE', *, *, #2773, .T. ) ;
#8749 = EDGE_LOOP ( 'NONE', ( #15920, #3084, #3461, #12124 ) ) ;
#8751 = EDGE_LOOP ( 'NONE', ( #9681, #8444, #22527, #21835 ) ) ;
#8753 = VERTEX_POINT ( 'NONE', #7204 ) ;
#8752 = ORIENTED_EDGE ( 'NONE', *, *, #16549, .F. ) ;
#8754 = AXIS2_PLACEMENT_3D ( 'NONE', #12836, #18138, #18253 ) ;
#8755 = ORIENTED_EDGE ( 'NONE', *, *, #7084, .F. ) ;
#8756 = VECTOR ( 'NONE', #3925, 1000.000000000000000 ) ;
#8757 = CIRCLE ( 'NONE', #4615, 5.999999999999998224 ) ;
#8758 = AXIS2_PLACEMENT_3D ( 'NONE', #2354, #6013, #5892 ) ;
#8759 = EDGE_LOOP ( 'NONE', ( #12057, #7796, #9685, #6606, #21468, #17605 ) ) ;
#8760 = LINE ( 'NONE', #17824, #15176 ) ;
#8761 = DIRECTION ( 'NONE',  ( 0.7071067811865457964, -0.7071067811865492381, 0.000000000000000000 ) ) ;
#8762 = VERTEX_POINT ( 'NONE', #1672 ) ;
#8763 = CARTESIAN_POINT ( 'NONE',  ( 1.369266385878517678, 0.000000000000000000, 0.000000000000000000 ) ) ;
#8764 = CARTESIAN_POINT ( 'NONE',  ( 0.000000000000000000, 0.000000000000000000, 0.000000000000000000 ) ) ;
#8765 = EDGE_CURVE ( 'NONE', #16716, #4023, #21554, .T. ) ;
#8766 = CARTESIAN_POINT ( 'NONE',  ( -2.449848172108612943, -3.432307619358808903, -3.503702292528934503 ) ) ;
#8767 = CARTESIAN_POINT ( 'NONE',  ( 4.630153689607049650, 0.000000000000000000, -3.469446951953614189E-15 ) ) ;
#8768 = CARTESIAN_POINT ( 'NONE',  ( -4.197393957002394593, -7.172049766556752605E-14, -3.503767560748959120 ) ) ;
#8769 = DIRECTION ( 'NONE',  ( -1.000000000000000000, -1.734723475976804728E-15, 0.000000000000000000 ) ) ;
#8770 = CARTESIAN_POINT ( 'NONE',  ( -6.959810536856680940, 36.00015702695179698, -26.48940942388196618 ) ) ;
#8771 = SURFACE_STYLE_FILL_AREA ( #4768 ) ;
#8772 = DIRECTION ( 'NONE',  ( 2.013525853228507892E-32, 6.902532920683810383E-31, -1.000000000000000000 ) ) ;
#8773 = CIRCLE ( 'NONE', #1633, 4.750000000000000888 ) ;
#8774 = CIRCLE ( 'NONE', #21929, 4.000000000000000000 ) ;
#8775 = DIRECTION ( 'NONE',  ( 1.000000000000000000, 3.254448077276381206E-32, 1.066788928082016908E-26 ) ) ;
#8776 = VECTOR ( 'NONE', #10346, 1000.000000000000000 ) ;
#8777 = CARTESIAN_POINT ( 'NONE',  ( -8.113551354209993960, -1.583389928980782457, 7.426820295479581446 ) ) ;
#8778 = CIRCLE ( 'NONE', #11379, 0.5000000000000049960 ) ;
#8779 = ORIENTED_EDGE ( 'NONE', *, *, #21882, .F. ) ;
#8780 = AXIS2_PLACEMENT_3D ( 'NONE', #346, #3974, #15024 ) ;
#8781 = CIRCLE ( 'NONE', #7947, 2.999999999999999112 ) ;
#8782 = FILL_AREA_STYLE ('',( #5129 ) ) ;
#8783 = DIRECTION ( 'NONE',  ( -8.438582421954109416E-32, 0.000000000000000000, -1.000000000000000000 ) ) ;
#8784 = DIRECTION ( 'NONE',  ( -3.885780586188016830E-16, -4.437342591868156373E-31, 1.000000000000000000 ) ) ;
#8786 = ORIENTED_EDGE ( 'NONE', *, *, #18570, .T. ) ;
#8785 = ORIENTED_EDGE ( 'NONE', *, *, #18878, .F. ) ;
#8787 = VERTEX_POINT ( 'NONE', #3558 ) ;
#8788 = ORIENTED_EDGE ( 'NONE', *, *, #20327, .F. ) ;
#8789 = ORIENTED_EDGE ( 'NONE', *, *, #17570, .T. ) ;
#8790 = EDGE_CURVE ( 'NONE', #14827, #5349, #8001, .T. ) ;
#8791 = DIRECTION ( 'NONE',  ( 0.000000000000000000, 0.000000000000000000, 1.000000000000000000 ) ) ;
#8792 = VECTOR ( 'NONE', #10076, 1000.000000000000000 ) ;
#8793 = AXIS2_PLACEMENT_3D ( 'NONE', #6517, #10042, #1225 ) ;
#8794 = DIRECTION ( 'NONE',  ( -0.6819983600624998088, -0.7313537016191693496, 0.000000000000000000 ) ) ;
#8795 = CONICAL_SURFACE ( 'NONE', #6920, 2.249999999999996003, 0.7853981633974439491 ) ;
#8796 = FACE_OUTER_BOUND ( 'NONE', #19702, .T. ) ;
#8797 = CARTESIAN_POINT ( 'NONE',  ( 4.082498951862915781, -2.020725942163695166, -3.500000000000000444 ) ) ;
#8798 = EDGE_CURVE ( 'NONE', #8024, #7652, #23044, .T. ) ;
#8799 = CARTESIAN_POINT ( 'NONE',  ( 2.918498775983380256E-10, 2.999999999003851503, 0.000000000000000000 ) ) ;
#8800 = DIRECTION ( 'NONE',  ( 1.000000000000000000, -4.190823558986610327E-31, 1.733449886265890494E-32 ) ) ;
#8801 = FACE_OUTER_BOUND ( 'NONE', #20663, .T. ) ;
#8802 = FACE_OUTER_BOUND ( 'NONE', #1754, .T. ) ;
#8803 = DIRECTION ( 'NONE',  ( 1.000000000000000000, 2.699383410053119644E-30, 3.330669073875432643E-16 ) ) ;
#8804 = CARTESIAN_POINT ( 'NONE',  ( 37.09721192198001916, 10.82270004028415933, -10.48161866288213240 ) ) ;
#8805 = EDGE_CURVE ( 'NONE', #19106, #13336, #20028, .T. ) ;
#8806 = EDGE_CURVE ( 'NONE', #9602, #4343, #21447, .T. ) ;
#8807 = DIRECTION ( 'NONE',  ( 8.438582421954110511E-32, 0.000000000000000000, 1.000000000000000000 ) ) ;
#8808 = DIRECTION ( 'NONE',  ( -2.775557561562883955E-17, 3.406761633869148826E-16, -1.000000000000000000 ) ) ;
#8809 = CARTESIAN_POINT ( 'NONE',  ( 0.1750025118120909495, 4.719839900820656631, -3.469254087858260505 ) ) ;
#8810 = AXIS2_PLACEMENT_3D ( 'NONE', #17079, #4963, #13688 ) ;
#8811 = DIRECTION ( 'NONE',  ( -1.066786462891689527E-26, -6.656013887802287108E-31, -1.000000000000000000 ) ) ;
#8812 = AXIS2_PLACEMENT_3D ( 'NONE', #23082, #8948, #12345 ) ;
#8813 = CARTESIAN_POINT ( 'NONE',  ( 2.775557561562891351E-14, 10.49999999999999822, -9.999999999999968026 ) ) ;
#8814 = ORIENTED_EDGE ( 'NONE', *, *, #16257, .T. ) ;
#8815 = AXIS2_PLACEMENT_3D ( 'NONE', #10403, #6759, #13822 ) ;
#8816 = EDGE_LOOP ( 'NONE', ( #13896, #10749, #14162, #15595 ) ) ;
#8817 = CARTESIAN_POINT ( 'NONE',  ( -50.65685424949270299, 7.200000000000025935, 7.500000000000062172 ) ) ;
#8818 = EDGE_CURVE ( 'NONE', #14256, #22384, #6639, .T. ) ;
#8819 = ADVANCED_FACE ( 'NONE', ( #8967 ), #9150, .T. ) ;
#8821 = ORIENTED_EDGE ( 'NONE', *, *, #15985, .T. ) ;
#8820 = ORIENTED_EDGE ( 'NONE', *, *, #3459, .F. ) ;
#8822 = CARTESIAN_POINT ( 'NONE',  ( 4.175648173966012955, -2.207990556236570701, -3.469390959564061294 ) ) ;
#8823 = FACE_OUTER_BOUND ( 'NONE', #1699, .T. ) ;
#8824 = LINE ( 'NONE', #12451, #8471 ) ;
#8825 = AXIS2_PLACEMENT_3D ( 'NONE', #13659, #6479, #17402 ) ;
#8826 = ORIENTED_EDGE ( 'NONE', *, *, #14274, .T. ) ;
#8827 = CARTESIAN_POINT ( 'NONE',  ( 0.3126073911696447549, -4.041451884327383226, 0.000000000000000000 ) ) ;
#8828 = CARTESIAN_POINT ( 'NONE',  ( 108.2426266706970353, -6.527605602963587828, 6.500000000000199840 ) ) ;
#8829 = ADVANCED_FACE ( 'NONE', ( #12362 ), #14366, .F. ) ;
#8830 = CARTESIAN_POINT ( 'NONE',  ( 7.270142102516842962E-25, -4.472841332603135502E-27, -7.499999999999998224 ) ) ;
#8831 = CARTESIAN_POINT ( 'NONE',  ( -7.028413389564965641, -13.36994781876315130, 8.946655872546031674 ) ) ;
#8832 = DIRECTION ( 'NONE',  ( -1.000000000000000000, 4.190823558986610327E-31, -1.733449886265890494E-32 ) ) ;
#8833 = CARTESIAN_POINT ( 'NONE',  ( 8.422565759993842605, -1.999999999999981792, 6.396710472006605919 ) ) ;
#8834 = EDGE_CURVE ( 'NONE', #5817, #9446, #23212, .T. ) ;
#8835 = FACE_OUTER_BOUND ( 'NONE', #21729, .T. ) ;
#8836 = PLANE ( 'NONE',  #18343 ) ;
#8838 = EDGE_CURVE ( 'NONE', #4291, #4366, #4239, .T. ) ;
#8837 = CARTESIAN_POINT ( 'NONE',  ( -4.690415759823429731, 0.7500000000000630607, -3.000000000000002665 ) ) ;
#8839 = CARTESIAN_POINT ( 'NONE',  ( 3.999999999999939160, 0.1981133338132110011, 4.941929027460484850E-14 ) ) ;
#8840 = FILL_AREA_STYLE_COLOUR ( '', #23256 ) ;
#8841 = ORIENTED_EDGE ( 'NONE', *, *, #18293, .T. ) ;
#8842 = AXIS2_PLACEMENT_3D ( 'NONE', #15383, #11969, #9990 ) ;
#8843 = VECTOR ( 'NONE', #13881, 1000.000000000000000 ) ;
#8845 = ORIENTED_EDGE ( 'NONE', *, *, #19046, .T. ) ;
#8844 = ORIENTED_EDGE ( 'NONE', *, *, #9603, .F. ) ;
#8846 = ADVANCED_FACE ( 'NONE', ( #5202 ), #4250, .F. ) ;
#8847 = ORIENTED_EDGE ( 'NONE', *, *, #13413, .F. ) ;
#8849 = ORIENTED_EDGE ( 'NONE', *, *, #21171, .T. ) ;
#8848 = ORIENTED_EDGE ( 'NONE', *, *, #17990, .T. ) ;
#8850 = DIRECTION ( 'NONE',  ( 0.000000000000000000, -0.000000000000000000, 1.000000000000000000 ) ) ;
#8851 = FACE_OUTER_BOUND ( 'NONE', #7372, .T. ) ;
#8852 = DIRECTION ( 'NONE',  ( 1.550910762415566494E-16, 1.000000000000000000, -8.135128085091684243E-31 ) ) ;
#8853 = CARTESIAN_POINT ( 'NONE',  ( -6.999999999708156118, 6.999999999003851947, -29.00000000000000355 ) ) ;
#8854 = DIRECTION ( 'NONE',  ( 0.000000000000000000, 0.000000000000000000, -1.000000000000000000 ) ) ;
#8855 = EDGE_CURVE ( 'NONE', #22680, #16775, #6142, .T. ) ;
#8856 = LINE ( 'NONE', #9430, #7535 ) ;
#8857 = CARTESIAN_POINT ( 'NONE',  ( 7.499999999999979572, -12.77629584335316437, 9.030675447289000957 ) ) ;
#8858 = CARTESIAN_POINT ( 'NONE',  ( -6.000000000000088818, 1.999999999999960032, -17.72029585817558228 ) ) ;
#8859 = DIRECTION ( 'NONE',  ( -2.013525853228507892E-32, -6.902532920683810383E-31, 1.000000000000000000 ) ) ;
#8860 = DIRECTION ( 'NONE',  ( -0.6819983600624989206, -0.7313537016191700157, 0.000000000000000000 ) ) ;
#8861 = DIRECTION ( 'NONE',  ( 3.330669073875457788E-16, 0.000000000000000000, -1.000000000000000000 ) ) ;
#8862 = ADVANCED_FACE ( 'NONE', ( #9194 ), #15875, .T. ) ;
#8863 = CARTESIAN_POINT ( 'NONE',  ( 12.84999999999997300, -1.499999999999997780, 1.387778780781445676E-14 ) ) ;
#8864 = AXIS2_PLACEMENT_3D ( 'NONE', #4226, #20602, #2474 ) ;
#8865 = CARTESIAN_POINT ( 'NONE',  ( 1.110223024625156540E-13, -1.750000000000001554, -4.750000000000000888 ) ) ;
#8866 = DIRECTION ( 'NONE',  ( 0.000000000000000000, 0.000000000000000000, -1.000000000000000000 ) ) ;
#8867 = CARTESIAN_POINT ( 'NONE',  ( -65.55642023346347003, 2.700000000000056577, -11.87813525200320797 ) ) ;
#8868 = EDGE_LOOP ( 'NONE', ( #11084, #10961, #3607, #21897 ) ) ;
#8870 = ORIENTED_EDGE ( 'NONE', *, *, #20624, .F. ) ;
#8869 = ORIENTED_EDGE ( 'NONE', *, *, #6942, .T. ) ;
#8871 = ORIENTED_EDGE ( 'NONE', *, *, #21894, .F. ) ;
#8873 = ORIENTED_EDGE ( 'NONE', *, *, #32, .T. ) ;
#8872 = ORIENTED_EDGE ( 'NONE', *, *, #21755, .F. ) ;
#8874 = ORIENTED_EDGE ( 'NONE', *, *, #764, .F. ) ;
#8875 = ORIENTED_EDGE ( 'NONE', *, *, #16953, .F. ) ;
#8876 = ORIENTED_EDGE ( 'NONE', *, *, #5784, .F. ) ;
#8877 = CYLINDRICAL_SURFACE ( 'NONE', #12940, 0.2500000000000002220 ) ;
#8878 = CIRCLE ( 'NONE', #2861, 5.500000000000046185 ) ;
#8879 = DIRECTION ( 'NONE',  ( -7.860214984770699307E-18, 1.409037165336591006E-16, 1.000000000000000000 ) ) ;
#8880 = ORIENTED_EDGE ( 'NONE', *, *, #6206, .F. ) ;
#8881 = EDGE_CURVE ( 'NONE', #15190, #17995, #2469, .T. ) ;
#8882 = CARTESIAN_POINT ( 'NONE',  ( -8.137537312224766950, -13.43749107754207017, 7.396067884835361816 ) ) ;
#8883 = CARTESIAN_POINT ( 'NONE',  ( 80.15235153779143218, -8.074585193523137860, -6.000000000000060396 ) ) ;
#8884 = VECTOR ( 'NONE', #20212, 1000.000000000000000 ) ;
#8885 = FACE_OUTER_BOUND ( 'NONE', #12447, .T. ) ;
#8886 = CARTESIAN_POINT ( 'NONE',  ( -6.958637146882876934, 36.00028510068597143, -26.49646658807206379 ) ) ;
#8887 = CARTESIAN_POINT ( 'NONE',  ( 0.02511973781845255188, -4.877415612947488377, -3.751298745799865664 ) ) ;
#8888 = SURFACE_STYLE_USAGE ( .BOTH. , #5601 ) ;
#8889 = EDGE_CURVE ( 'NONE', #15940, #16720, #5761, .T. ) ;
#8890 =( NAMED_UNIT ( * ) PLANE_ANGLE_UNIT ( ) SI_UNIT ( $, .RADIAN. ) );
#8891 = LINE ( 'NONE', #7021, #17997 ) ;
#8892 = DIRECTION ( 'NONE',  ( 0.000000000000000000, 0.000000000000000000, -1.000000000000000000 ) ) ;
#8893 = CARTESIAN_POINT ( 'NONE',  ( 3.000000000000002665, 2.499999999999998668, 2.775557561562891351E-14 ) ) ;
#8894 = ORIENTED_EDGE ( 'NONE', *, *, #13262, .F. ) ;
#8895 = AXIS2_PLACEMENT_3D ( 'NONE', #7697, #2394, #20286 ) ;
#8896 =( NAMED_UNIT ( * ) PLANE_ANGLE_UNIT ( ) SI_UNIT ( $, .RADIAN. ) );
#8897 = CARTESIAN_POINT ( 'NONE',  ( 77.42435809754145737, -3.999999999999809042, -6.499999999999984901 ) ) ;
#8898 = CARTESIAN_POINT ( 'NONE',  ( -4.197393957002394593, -7.172049766556752605E-14, -3.503767560748959120 ) ) ;
#8900 = ORIENTED_EDGE ( 'NONE', *, *, #7419, .T. ) ;
#8899 = ORIENTED_EDGE ( 'NONE', *, *, #1966, .T. ) ;
#8901 = AXIS2_PLACEMENT_3D ( 'NONE', #15815, #7023, #17838 ) ;
#8902 = ADVANCED_FACE ( 'NONE', ( #7542 ), #21912, .T. ) ;
#8903 = ORIENTED_EDGE ( 'NONE', *, *, #456, .F. ) ;
#8904 = ORIENTED_EDGE ( 'NONE', *, *, #17112, .F. ) ;
#8905 = AXIS2_PLACEMENT_3D ( 'NONE', #12379, #10505, #14382 ) ;
#8906 = VERTEX_POINT ( 'NONE', #14704 ) ;
#8907 = EDGE_LOOP ( 'NONE', ( #1187, #17066, #15245, #20711 ) ) ;
#8908 = LINE ( 'NONE', #1611, #13665 ) ;
#8909 = CARTESIAN_POINT ( 'NONE',  ( 116.8476484622116232, -8.074585193523331483, 6.500000000000040856 ) ) ;
#8910 = CARTESIAN_POINT ( 'NONE',  ( 1.849731447993477218, -1.560358803165485586, 4.749999999999999112 ) ) ;
#8911 = CARTESIAN_POINT ( 'NONE',  ( 42.00000000000020606, 8.000000000000003553, -0.4999999999999449329 ) ) ;
#8912 = CARTESIAN_POINT ( 'NONE',  ( 66.26395429947831417, -4.000000000000003553, 6.000000000000192735 ) ) ;
#8913 = CARTESIAN_POINT ( 'NONE',  ( -47.82842712474646873, -4.371572875253880497, -7.500000000000034639 ) ) ;
#8914 = FACE_OUTER_BOUND ( 'NONE', #2039, .T. ) ;
#8915 = CARTESIAN_POINT ( 'NONE',  ( 0.000000000000000000, 0.000000000000000000, 0.000000000000000000 ) ) ;
#8916 = CIRCLE ( 'NONE', #17156, 2.500000000000014655 ) ;
#8917 = FACE_OUTER_BOUND ( 'NONE', #15349, .T. ) ;
#8918 = CARTESIAN_POINT ( 'NONE',  ( -66.55000000000046612, -7.593235069856354823E-14, -2.000000000000001776 ) ) ;
#8919 = AXIS2_PLACEMENT_3D ( 'NONE', #15182, #14720, #22377 ) ;
#8920 = FACE_BOUND ( 'NONE', #5697, .T. ) ;
#8921 = CARTESIAN_POINT ( 'NONE',  ( 24.75000000000001776, 0.2500000000000418554, -2.081668171172168513E-14 ) ) ;
#8922 = SURFACE_STYLE_FILL_AREA ( #7169 ) ;
#8923 = EDGE_CURVE ( 'NONE', #11150, #12860, #16352, .T. ) ;
#8924 = CIRCLE ( 'NONE', #4022, 2.550000000000024691 ) ;
#8925 = DIRECTION ( 'NONE',  ( 1.333893503340774882E-15, 2.778352770573747380E-17, 1.000000000000000000 ) ) ;
#8926 = CARTESIAN_POINT ( 'NONE',  ( 4.050536630291683871, -2.401306687817038821, 2.976670123173771554 ) ) ;
#8927 = VERTEX_POINT ( 'NONE', #16570 ) ;
#8928 = ADVANCED_FACE ( 'NONE', ( #13304 ), #5671, .T. ) ;
#8929 = VERTEX_POINT ( 'NONE', #13184 ) ;
#8930 = AXIS2_PLACEMENT_3D ( 'NONE', #22110, #6002, #20342 ) ;
#8931 = VECTOR ( 'NONE', #20215, 1000.000000000000000 ) ;
#8932 = CARTESIAN_POINT ( 'NONE',  ( -6.975867733732471265, 36.00005661733526807, -26.49364064955104681 ) ) ;
#8934 = EDGE_CURVE ( 'NONE', #10146, #16720, #14785, .T. ) ;
#8933 = EDGE_LOOP ( 'NONE', ( #4752, #8725, #2186, #2031 ) ) ;
#8935 = AXIS2_PLACEMENT_3D ( 'NONE', #21765, #125, #15862 ) ;
#8936 = DIRECTION ( 'NONE',  ( 2.220446049250313081E-16, -1.000000000000000000, 7.025792437124636392E-31 ) ) ;
#8937 = ADVANCED_FACE ( 'NONE', ( #22006 ), #5787, .T. ) ;
#8938 = CARTESIAN_POINT ( 'NONE',  ( 3.999999999999948042, 2.309401076758532678, -5.000000000000000888 ) ) ;
#8939 = CARTESIAN_POINT ( 'NONE',  ( 42.50000000000014921, 8.000000000000003553, -12.49999999999998401 ) ) ;
#8940 = CARTESIAN_POINT ( 'NONE',  ( 54.42435809754115894, 2.999999999999947153, -5.999999999999950262 ) ) ;
#8941 = EDGE_LOOP ( 'NONE', ( #8848, #11487 ) ) ;
#8942 = DIRECTION ( 'NONE',  ( 5.551115123125818447E-17, -1.577721810442025713E-30, 1.000000000000000000 ) ) ;
#8943 = CARTESIAN_POINT ( 'NONE',  ( 114.8016533820240426, -5.880524088665822546, 6.500000000000123457 ) ) ;
#8944 = CARTESIAN_POINT ( 'NONE',  ( 7.938566201357313723, 4.882486540518877760, -1.249999999999957145 ) ) ;
#8945 = DIRECTION ( 'NONE',  ( -2.172745813409349776E-17, 1.000000000000000000, -1.309377075419428048E-16 ) ) ;
#8946 = DIRECTION ( 'NONE',  ( 8.438582421954110511E-32, 0.000000000000000000, 1.000000000000000000 ) ) ;
#8947 = DIRECTION ( 'NONE',  ( 0.000000000000000000, 0.000000000000000000, -1.000000000000000000 ) ) ;
#8948 = DIRECTION ( 'NONE',  ( -1.000000000000000000, -3.254448077276381206E-32, -1.066788928082016908E-26 ) ) ;
#8949 = DIRECTION ( 'NONE',  ( -1.000000000000000000, -3.254448077276381206E-32, -1.066788928082016908E-26 ) ) ;
#8950 = SURFACE_STYLE_FILL_AREA ( #12706 ) ;
#8951 = CIRCLE ( 'NONE', #13832, 2.250000000000001776 ) ;
#8952 = EDGE_CURVE ( 'NONE', #4310, #14732, #7429, .T. ) ;
#8953 = ADVANCED_FACE ( 'NONE', ( #9649 ), #11063, .T. ) ;
#8954 = CARTESIAN_POINT ( 'NONE',  ( -4.000000000000045297, 1.387778780781445676E-14, 0.000000000000000000 ) ) ;
#8955 = VERTEX_POINT ( 'NONE', #20125 ) ;
#8956 = ADVANCED_FACE ( 'NONE', ( #16802 ), #7886, .T. ) ;
#8957 = AXIS2_PLACEMENT_3D ( 'NONE', #11746, #4697, #6695 ) ;
#8958 = APPLICATION_PROTOCOL_DEFINITION ( 'draft international standard', 'automotive_design', 1998, #19150 ) ;
#8959 = B_SPLINE_CURVE_WITH_KNOTS ( 'NONE', 3,
 ( #1221, #8399, #6514, #10039 ),
 .UNSPECIFIED., .F., .F.,
 ( 4, 4 ),
 ( 0.000000000000000000, 0.002080789711329279756 ),
 .UNSPECIFIED. ) ;
#8960 = AXIS2_PLACEMENT_3D ( 'NONE', #11771, #19298, #20726 ) ;
#8962 = VERTEX_POINT ( 'NONE', #11290 ) ;
#8961 = ORIENTED_EDGE ( 'NONE', *, *, #16881, .T. ) ;
#8963 = ORIENTED_EDGE ( 'NONE', *, *, #393, .F. ) ;
#8966 = EDGE_LOOP ( 'NONE', ( #3411, #6711, #17573, #17677, #20739, #11819, #6762 ) ) ;
#8965 = ADVANCED_FACE ( 'NONE', ( #11181 ), #485, .F. ) ;
#8964 = VERTEX_POINT ( 'NONE', #4000 ) ;
#8967 = FACE_OUTER_BOUND ( 'NONE', #20657, .T. ) ;
#8968 =( GEOMETRIC_REPRESENTATION_CONTEXT ( 3 ) GLOBAL_UNCERTAINTY_ASSIGNED_CONTEXT ( ( #7908 ) ) GLOBAL_UNIT_ASSIGNED_CONTEXT ( ( #7850, #18663, #2548 ) ) REPRESENTATION_CONTEXT ( 'NONE', 'WORKASPACE' ) );
#8969 = CARTESIAN_POINT ( 'NONE',  ( -10.49999999999998224, -0.5000000000000038858, 6.250000000000061284 ) ) ;
#8970 = LINE ( 'NONE', #17795, #7731 ) ;
#8971 = VECTOR ( 'NONE', #16927, 1000.000000000000227 ) ;
#8972 = DIRECTION ( 'NONE',  ( 0.000000000000000000, 0.000000000000000000, 1.000000000000000000 ) ) ;
#8973 = DIRECTION ( 'NONE',  ( 0.000000000000000000, 0.000000000000000000, -1.000000000000000000 ) ) ;
#8974 = CARTESIAN_POINT ( 'NONE',  ( 22.49999999999992539, 1.999999999999960032, -19.00000000000001421 ) ) ;
#8975 = AXIS2_PLACEMENT_3D ( 'NONE', #7851, #11024, #18217 ) ;
#8976 = FACE_OUTER_BOUND ( 'NONE', #10002, .T. ) ;
#8977 = CARTESIAN_POINT ( 'NONE',  ( 3.997250504095354984, 1.749999999999999556, -2.576559036326556917 ) ) ;
#8978 = VECTOR ( 'NONE', #23007, 1000.000000000000000 ) ;
#8979 = DIRECTION ( 'NONE',  ( 0.000000000000000000, 0.000000000000000000, 1.000000000000000000 ) ) ;
#8980 = CARTESIAN_POINT ( 'NONE',  ( 4.692963726980105221, -1.672424706883760326, -1.371548386792676766 ) ) ;
#8981 = EDGE_CURVE ( 'NONE', #19728, #19565, #22238, .T. ) ;
#8982 = DIRECTION ( 'NONE',  ( -1.858632295689435609E-16, -1.000000000000000000, 2.999267978177796234E-32 ) ) ;
#8983 = EDGE_CURVE ( 'NONE', #6938, #23124, #523, .T. ) ;
#8984 = LINE ( 'NONE', #7115, #19837 ) ;
#8985 = CARTESIAN_POINT ( 'NONE',  ( 1.387778780781445676E-14, 4.163336342344337027E-14, -2.000000000000001776 ) ) ;
#8986 = CARTESIAN_POINT ( 'NONE',  ( 7.991520206789727965, -0.6043476454135817688, 7.599114430427888145 ) ) ;
#8987 = ORIENTED_EDGE ( 'NONE', *, *, #4369, .T. ) ;
#8989 = ORIENTED_EDGE ( 'NONE', *, *, #12969, .T. ) ;
#8988 = VERTEX_POINT ( 'NONE', #11757 ) ;
#8990 = EDGE_CURVE ( 'NONE', #14077, #4310, #6245, .T. ) ;
#8991 = VERTEX_POINT ( 'NONE', #2828 ) ;
#8992 = CIRCLE ( 'NONE', #16864, 2.250000000000001776 ) ;
#8994 = ORIENTED_EDGE ( 'NONE', *, *, #19686, .T. ) ;
#8993 = ORIENTED_EDGE ( 'NONE', *, *, #13223, .T. ) ;
#8995 = AXIS2_PLACEMENT_3D ( 'NONE', #14185, #3377, #19590 ) ;
#8996 = AXIS2_PLACEMENT_3D ( 'NONE', #3833, #19963, #4294 ) ;
#8997 = ORIENTED_EDGE ( 'NONE', *, *, #16109, .F. ) ;
#8998 = EDGE_LOOP ( 'NONE', ( #16030, #5132, #11955, #6702 ) ) ;
#8999 = VERTEX_POINT ( 'NONE', #18821 ) ;
#9000 = CARTESIAN_POINT ( 'NONE',  ( 66.26395429947837101, -4.000000000000003553, 6.500000000000110134 ) ) ;
#9001 = AXIS2_PLACEMENT_3D ( 'NONE', #21537, #351, #234 ) ;
#9002 = DIRECTION ( 'NONE',  ( 2.172745813409349776E-17, -1.000000000000000000, 1.309377075419428048E-16 ) ) ;
#9003 = CARTESIAN_POINT ( 'NONE',  ( -8.502135871254331789, -13.49242826152325492, 6.995667647939170841 ) ) ;
#9004 = DIRECTION ( 'NONE',  ( -5.551115123125782702E-16, -1.201780285297635172E-31, 1.000000000000000000 ) ) ;
#9005 = CARTESIAN_POINT ( 'NONE',  ( 88.75737332930592061, -6.527605602963476805, -6.000000000000012434 ) ) ;
#9006 = CARTESIAN_POINT ( 'NONE',  ( -10.49999999999996803, -12.50000000000002842, 5.750000000000060396 ) ) ;
#9007 = CARTESIAN_POINT ( 'NONE',  ( -4.235886605889470857, -2.417314728048573169, -3.751161874094045334 ) ) ;
#9008 = DIRECTION ( 'NONE',  ( -2.220446049250313081E-16, 1.000000000000000000, -7.025792437124636392E-31 ) ) ;
#9009 = FACE_OUTER_BOUND ( 'NONE', #18051, .T. ) ;
#9010 = CARTESIAN_POINT ( 'NONE',  ( -65.47859922179024750, -3.200000000000088107, -11.38422848940301435 ) ) ;
#9011 = CARTESIAN_POINT ( 'NONE',  ( -7.713464495931991571, -1.828647720521560327, 8.131426806228610360 ) ) ;
#9012 = EDGE_LOOP ( 'NONE', ( #22306, #14757, #4463, #4815 ) ) ;
#9013 = DIRECTION ( 'NONE',  ( 1.000000000000000000, 1.503427012513217564E-14, 3.854941057726199147E-16 ) ) ;
#9014 = DIRECTION ( 'NONE',  ( 1.000000000000000000, 2.220446049250313081E-16, 3.469446951953592101E-15 ) ) ;
#9015 = VECTOR ( 'NONE', #13069, 1000.000000000000000 ) ;
#9017 = ORIENTED_EDGE ( 'NONE', *, *, #22824, .T. ) ;
#9016 = ORIENTED_EDGE ( 'NONE', *, *, #20482, .T. ) ;
#9018 = STYLED_ITEM ( 'NONE', ( #2376 ), #15637 ) ;
#9019 = ORIENTED_EDGE ( 'NONE', *, *, #22283, .F. ) ;
#9020 = B_SPLINE_CURVE_WITH_KNOTS ( 'NONE', 3,
 ( #13568, #17547, #4736, #8042, #4505, #11672 ),
 .UNSPECIFIED., .F., .F.,
 ( 4, 2, 4 ),
 ( 0.002336974151641583747, 0.003500975885716454093, 0.004664977619791324873 ),
 .UNSPECIFIED. ) ;
#9021 = ORIENTED_EDGE ( 'NONE', *, *, #8539, .F. ) ;
#9022 = ADVANCED_FACE ( 'NONE', ( #6469 ), #10004, .T. ) ;
#9023 = ORIENTED_EDGE ( 'NONE', *, *, #23227, .T. ) ;
#9024 = CYLINDRICAL_SURFACE ( 'NONE', #20817, 7.000000000000006217 ) ;
#9025 = CYLINDRICAL_SURFACE ( 'NONE', #4595, 2.500000000000015543 ) ;
#9026 = CARTESIAN_POINT ( 'NONE',  ( 25.60000000000000142, 2.789133085058096608E-16, -2.055000000000006821 ) ) ;
#9027 = CARTESIAN_POINT ( 'NONE',  ( 3.972709601346593455, 3.429395227388313927, 1.191688283765304890 ) ) ;
#9028 = DIRECTION ( 'NONE',  ( 0.000000000000000000, 0.000000000000000000, 1.000000000000000000 ) ) ;
#9029 = FACE_OUTER_BOUND ( 'NONE', #13670, .T. ) ;
#9030 = AXIS2_PLACEMENT_3D ( 'NONE', #16734, #12871, #12991 ) ;
#9031 = CARTESIAN_POINT ( 'NONE',  ( 7.595478965369733437, -11.97605770252014246, 8.489833260407458226 ) ) ;
#9032 = CARTESIAN_POINT ( 'NONE',  ( 77.42435809754137210, -4.499999999999809930, -5.999999999999984901 ) ) ;
#9033 = CARTESIAN_POINT ( 'NONE',  ( 42.50000000000020606, 2.499999999999998668, -13.00000000000002487 ) ) ;
#9034 = DIRECTION ( 'NONE',  ( 1.000000000000000000, 6.224605580259554159E-31, -2.887593071917436153E-31 ) ) ;
#9035 = DIRECTION ( 'NONE',  ( -0.7071067811865485719, 0.7071067811865464625, 1.010793663541191485E-16 ) ) ;
#9036 = DIRECTION ( 'NONE',  ( -1.000000000000000000, 0.000000000000000000, 0.000000000000000000 ) ) ;
#9037 = DIRECTION ( 'NONE',  ( -1.000000000000000000, 4.615739097524200579E-16, -1.134196829589822059E-15 ) ) ;
#9038 = DIRECTION ( 'NONE',  ( 1.000000000000000000, 0.000000000000000000, 0.000000000000000000 ) ) ;
#9039 = CARTESIAN_POINT ( 'NONE',  ( -0.6507732100474116210, 4.243078065514748864, -0.2236248678334617213 ) ) ;
#9040 = VERTEX_POINT ( 'NONE', #4817 ) ;
#9041 = AXIS2_PLACEMENT_3D ( 'NONE', #22395, #2507, #758 ) ;
#9042 = ORIENTED_EDGE ( 'NONE', *, *, #14392, .F. ) ;
#9043 = CARTESIAN_POINT ( 'NONE',  ( -5.403531933167076140, 36.45753077221091587, -28.65347769269738976 ) ) ;
#9044 = ORIENTED_EDGE ( 'NONE', *, *, #14260, .F. ) ;
#9045 = CARTESIAN_POINT ( 'NONE',  ( -3.646393709166010577, 1.750000000000053291, -3.184260831324756680 ) ) ;
#9046 = CARTESIAN_POINT ( 'NONE',  ( 83.98338480886823731, -11.64708151429766403, 6.500000000000117240 ) ) ;
#9047 = CARTESIAN_POINT ( 'NONE',  ( 0.000000000000000000, 1.750000000000001554, 0.000000000000000000 ) ) ;
#9048 = ORIENTED_EDGE ( 'NONE', *, *, #15249, .F. ) ;
#9049 = CARTESIAN_POINT ( 'NONE',  ( 6.495190528383244732, 4.999999999999948486, -3.750000000000000000 ) ) ;
#9050 = CARTESIAN_POINT ( 'NONE',  ( 4.071447262713884463, -4.041451884327383226, 0.000000000000000000 ) ) ;
#9051 = DIRECTION ( 'NONE',  ( 0.000000000000000000, 0.000000000000000000, 1.000000000000000000 ) ) ;
#9052 = CARTESIAN_POINT ( 'NONE',  ( -7.126417736726679664, -13.56697759857014596, 8.494066294656329674 ) ) ;
#9053 = EDGE_CURVE ( 'NONE', #6614, #19105, #17043, .T. ) ;
#9054 = CARTESIAN_POINT ( 'NONE',  ( 42.50000000000014921, 2.999999999999999112, -12.49999999999998401 ) ) ;
#9055 = DIRECTION ( 'NONE',  ( 0.000000000000000000, 0.000000000000000000, -1.000000000000000000 ) ) ;
#9056 = CIRCLE ( 'NONE', #18440, 7.499999999999998224 ) ;
#9057 = AXIS2_PLACEMENT_3D ( 'NONE', #9840, #11708, #18899 ) ;
#9058 = DIRECTION ( 'NONE',  ( -4.190823558986625216E-31, 1.000000000000000000, -4.190823558986625216E-31 ) ) ;
#9059 = CARTESIAN_POINT ( 'NONE',  ( 3.972066048304704555, -2.740530939476112149, 2.384802634787816622 ) ) ;
#9060 = CARTESIAN_POINT ( 'NONE',  ( -3.499999999708153453, 35.49999999900384751, -19.50000000000000355 ) ) ;
#9061 = CARTESIAN_POINT ( 'NONE',  ( 0.1381419387168565938, -1.355287006802375460, 3.499999999999994227 ) ) ;
#9062 = ORIENTED_EDGE ( 'NONE', *, *, #17515, .F. ) ;
#9064 = ORIENTED_EDGE ( 'NONE', *, *, #22623, .T. ) ;
#9063 = EDGE_LOOP ( 'NONE', ( #5846, #6158, #5460, #9330 ) ) ;
#9065 = B_SPLINE_CURVE_WITH_KNOTS ( 'NONE', 3,
 ( #15885, #4845, #19200, #6848 ),
 .UNSPECIFIED., .F., .F.,
 ( 4, 4 ),
 ( 0.000000000000000000, 0.002452478801916411870 ),
 .UNSPECIFIED. ) ;
#9066 = ORIENTED_EDGE ( 'NONE', *, *, #19882, .T. ) ;
#9068 = EDGE_LOOP ( 'NONE', ( #13125, #627, #15650, #3007 ) ) ;
#9067 = VERTEX_POINT ( 'NONE', #11986 ) ;
#9069 = AXIS2_PLACEMENT_3D ( 'NONE', #14321, #1731, #19741 ) ;
#9070 = CARTESIAN_POINT ( 'NONE',  ( -0.1756481739660878671, 4.720212674039040657, -3.469390959564085719 ) ) ;
#9071 = CARTESIAN_POINT ( 'NONE',  ( 37.00000000000027711, 0.2500000000000007216, -2.566987298107707982 ) ) ;
#9072 = ADVANCED_FACE ( 'NONE', ( #8004 ), #10221, .F. ) ;
#9073 = CARTESIAN_POINT ( 'NONE',  ( 7.835522544085312902, -11.94917567266014480, 6.894286109559232045 ) ) ;
#9074 =( BOUNDED_SURFACE ( )  B_SPLINE_SURFACE ( 3, 2, ( 
 ( #11674, #6403, #7925 ),
 ( #6173, #15326, #18985 ),
 ( #9929, #13572, #2862 ),
 ( #13690, #19093, #15205 ),
 ( #17202, #9807, #1114 ),
 ( #4620, #4509, #647 ) ),
 .UNSPECIFIED., .F., .F., .T. ) 
 B_SPLINE_SURFACE_WITH_KNOTS ( ( 4, 2, 4 ),
 ( 3, 3 ),
 ( 0.02027065861071770947, 0.02273072267836921678, 0.02519078674602072410 ),
 ( 0.000000000000000000, 1.000000000000000000 ),
 .UNSPECIFIED. ) 
 GEOMETRIC_REPRESENTATION_ITEM ( )  RATIONAL_B_SPLINE_SURFACE ( (
 ( 1.000000000000000000, 0.8047781708337304885, 1.000000000000000000),
 ( 1.000000000000000000, 0.8123765190705294348, 1.000000000000000000),
 ( 1.000000000000000000, 0.8190656277163984589, 1.000000000000000000),
 ( 1.000000000000000000, 0.8192366903512168230, 1.000000000000000000),
 ( 1.000000000000000000, 0.8126138454302894720, 1.000000000000000000),
 ( 1.000000000000000000, 0.8047712246031424321, 1.000000000000000000) ) ) 
 REPRESENTATION_ITEM ( '' )  SURFACE ( )  );
#9075 = FACE_OUTER_BOUND ( 'NONE', #19286, .T. ) ;
#9076 = CARTESIAN_POINT ( 'NONE',  ( -2.109645605488527628E-31, -1.750000000000001554, -2.500000000000000000 ) ) ;
#9077 = CARTESIAN_POINT ( 'NONE',  ( 8.223343937052064234, -13.45452499186315265, 7.291631794411112644 ) ) ;
#9078 = ADVANCED_FACE ( 'NONE', ( #957 ), #8240, .F. ) ;
#9079 = DIRECTION ( 'NONE',  ( 1.550910762415566494E-16, 1.000000000000000000, -8.135128085091684243E-31 ) ) ;
#9080 = CARTESIAN_POINT ( 'NONE',  ( 3.000000000291852764, 42.99999999900385461, -26.50000000000000000 ) ) ;
#9081 = LINE ( 'NONE', #9202, #15892 ) ;
#9082 = FACE_OUTER_BOUND ( 'NONE', #7595, .T. ) ;
#9083 = APPLICATION_CONTEXT ( 'automotive_design' ) ;
#9084 = DIRECTION ( 'NONE',  ( 0.000000000000000000, 0.000000000000000000, -1.000000000000000000 ) ) ;
#9085 = DIRECTION ( 'NONE',  ( -2.013525853228518840E-32, 6.779273404243028164E-31, -1.000000000000000000 ) ) ;
#9086 = ADVANCED_FACE ( 'NONE', ( #2947 ), #20049, .T. ) ;
#9087 = PLANE ( 'NONE',  #16799 ) ;
#9088 = AXIS2_PLACEMENT_3D ( 'NONE', #16526, #435, #21967 ) ;
#9089 = AXIS2_PLACEMENT_3D ( 'NONE', #9276, #6097, #18100 ) ;
#9090 = EDGE_CURVE ( 'NONE', #12443, #22242, #13299, .T. ) ;
#9091 = CARTESIAN_POINT ( 'NONE',  ( 0.000000000000000000, 0.000000000000000000, 0.000000000000000000 ) ) ;
#9092 = CARTESIAN_POINT ( 'NONE',  ( -43.46238456605041023, -4.919238815542528620, -7.500000000000007105 ) ) ;
#9093 = VERTEX_POINT ( 'NONE', #4706 ) ;
#9094 =( LENGTH_UNIT ( ) NAMED_UNIT ( * ) SI_UNIT ( .MILLI., .METRE. ) );
#9096 = ORIENTED_EDGE ( 'NONE', *, *, #5182, .T. ) ;
#9095 = ORIENTED_EDGE ( 'NONE', *, *, #22846, .F. ) ;
#9097 = UNCERTAINTY_MEASURE_WITH_UNIT (LENGTH_MEASURE( 1.000000000000000082E-05 ), #5214, 'distance_accuracy_value', 'NONE');
#9098 = VERTEX_POINT ( 'NONE', #6706 ) ;
#9100 = VERTEX_POINT ( 'NONE', #15516 ) ;
#9099 = ORIENTED_EDGE ( 'NONE', *, *, #877, .T. ) ;
#9101 = ORIENTED_EDGE ( 'NONE', *, *, #10964, .F. ) ;
#9102 = CARTESIAN_POINT ( 'NONE',  ( 4.175326769692856210, 2.060699556488912343, 3.569236330973476701 ) ) ;
#9103 = EDGE_CURVE ( 'NONE', #11691, #6938, #18704, .T. ) ;
#9104 = ORIENTED_EDGE ( 'NONE', *, *, #14098, .F. ) ;
#9105 = VERTEX_POINT ( 'NONE', #1183 ) ;
#9106 = ADVANCED_FACE ( 'NONE', ( #9768 ), #22364, .F. ) ;
#9107 = CARTESIAN_POINT ( 'NONE',  ( -2.249999999999996003, 2.875477633779155440E-14, 17.49999999999997513 ) ) ;
#9108 = ADVANCED_FACE ( 'NONE', ( #22709 ), #23060, .T. ) ;
#9109 = AXIS2_PLACEMENT_3D ( 'NONE', #17490, #13744, #10096 ) ;
#9110 = VECTOR ( 'NONE', #21152, 1000.000000000000000 ) ;
#9111 = CARTESIAN_POINT ( 'NONE',  ( -6.000000000000088818, -8.000000000000042633, 8.000000000000062172 ) ) ;
#9112 = AXIS2_PLACEMENT_3D ( 'NONE', #17107, #9836, #15352 ) ;
#9113 = DIRECTION ( 'NONE',  ( 0.000000000000000000, 0.000000000000000000, 1.000000000000000000 ) ) ;
#9114 = DIRECTION ( 'NONE',  ( 0.1556420233463076119, 0.000000000000000000, 0.9878135252003121813 ) ) ;
#9115 = CARTESIAN_POINT ( 'NONE',  ( 4.071447262713891568, -2.020725942163709377, -3.499999999999999556 ) ) ;
#9116 = LINE ( 'NONE', #15929, #11010 ) ;
#9117 = ADVANCED_FACE ( 'NONE', ( #13533 ), #6592, .F. ) ;
#9118 = LINE ( 'NONE', #7141, #15507 ) ;
#9119 = CARTESIAN_POINT ( 'NONE',  ( 1.044713074591974287E-14, -2.686816014504604944, -2.346298152288348593 ) ) ;
#9120 = EDGE_CURVE ( 'NONE', #10391, #19811, #3524, .T. ) ;
#9121 = COLOUR_RGB ( '', 0.72549020, 0.75294118, 0.79215686) ;
#9122 = DIRECTION ( 'NONE',  ( 1.000000000000000000, -1.389842848855773367E-62, 2.013525853228507618E-32 ) ) ;
#9123 = DIRECTION ( 'NONE',  ( 2.013525853228507892E-32, 6.902532920683810383E-31, -1.000000000000000000 ) ) ;
#9124 = ORIENTED_EDGE ( 'NONE', *, *, #13555, .T. ) ;
#9125 = PRODUCT_DEFINITION_CONTEXT ( 'detailed design', #7443, 'design' ) ;
#9126 = DIRECTION ( 'NONE',  ( 1.000000000000000000, 0.000000000000000000, 0.000000000000000000 ) ) ;
#9127 = DIRECTION ( 'NONE',  ( 0.000000000000000000, 0.000000000000000000, -1.000000000000000000 ) ) ;
#9128 = TOROIDAL_SURFACE ( 'NONE', #8738, 5.500000000000007994, 0.5000000000000000000 ) ;
#9130 = ORIENTED_EDGE ( 'NONE', *, *, #18929, .F. ) ;
#9129 = ORIENTED_EDGE ( 'NONE', *, *, #22669, .F. ) ;
#9131 = CIRCLE ( 'NONE', #1241, 0.8000000000000090372 ) ;
#9132 = AXIS2_PLACEMENT_3D ( 'NONE', #17583, #3471, #10640 ) ;
#9133 = VECTOR ( 'NONE', #5141, 1000.000000000000000 ) ;
#9134 = VERTEX_POINT ( 'NONE', #21061 ) ;
#9135 = ORIENTED_EDGE ( 'NONE', *, *, #14707, .F. ) ;
#9136 = ORIENTED_EDGE ( 'NONE', *, *, #6066, .T. ) ;
#9137 = EDGE_LOOP ( 'NONE', ( #8785, #8786, #2646, #19928 ) ) ;
#9138 = DIRECTION ( 'NONE',  ( 0.000000000000000000, 0.000000000000000000, -1.000000000000000000 ) ) ;
#9139 = DIRECTION ( 'NONE',  ( 0.8660254037844387076, -2.506296930348933473E-16, -0.4999999999999998335 ) ) ;
#9140 = DIRECTION ( 'NONE',  ( -1.000000000000000000, 0.000000000000000000, -4.336808689941968432E-16 ) ) ;
#9141 = VECTOR ( 'NONE', #11742, 1000.000000000000000 ) ;
#9142 = DIRECTION ( 'NONE',  ( -2.013525853228507892E-32, -6.902532920683810383E-31, 1.000000000000000000 ) ) ;
#9143 = CIRCLE ( 'NONE', #7272, 3.000000000000011102 ) ;
#9144 = DIRECTION ( 'NONE',  ( 0.000000000000000000, 0.000000000000000000, -1.000000000000000000 ) ) ;
#9145 = CARTESIAN_POINT ( 'NONE',  ( -7.499999999999992895, -8.000000000000044409, 6.250000000000005329 ) ) ;
#9146 = CIRCLE ( 'NONE', #14782, 2.099999999999999645 ) ;
#9147 = EDGE_CURVE ( 'NONE', #9714, #4863, #16287, .T. ) ;
#9148 = AXIS2_PLACEMENT_3D ( 'NONE', #5217, #17803, #15898 ) ;
#9149 = CARTESIAN_POINT ( 'NONE',  ( -6.938893903907228378E-14, 4.999999999999976907, -4.163336342344337027E-14 ) ) ;
#9150 = CONICAL_SURFACE ( 'NONE', #14403, 7.500000000000001776, 1.308996938995750092 ) ;
#9151 = AXIS2_PLACEMENT_3D ( 'NONE', #1782, #7101, #7207 ) ;
#9152 = CARTESIAN_POINT ( 'NONE',  ( -7.694134585029390294, -13.68800912542550385, 8.172315317061205064 ) ) ;
#9153 = CARTESIAN_POINT ( 'NONE',  ( -42.54314575050793934, -4.000000000000021316, 7.500000000000062172 ) ) ;
#9154 = DIRECTION ( 'NONE',  ( 3.330669073875432643E-16, 4.437342591868153746E-31, -1.000000000000000000 ) ) ;
#9155 = FACE_OUTER_BOUND ( 'NONE', #14625, .T. ) ;
#9156 = CARTESIAN_POINT ( 'NONE',  ( 37.04362427881591202, 0.2122202663360315822, -10.45482484129306400 ) ) ;
#9157 = EDGE_CURVE ( 'NONE', #8787, #18266, #7723, .T. ) ;
#9158 = DIRECTION ( 'NONE',  ( 1.000000000000000000, 0.000000000000000000, 0.000000000000000000 ) ) ;
#9159 = FACE_OUTER_BOUND ( 'NONE', #9940, .T. ) ;
#9160 = VERTEX_POINT ( 'NONE', #19521 ) ;
#9161 = AXIS2_PLACEMENT_3D ( 'NONE', #5483, #20371, #9122 ) ;
#9162 = CIRCLE ( 'NONE', #13295, 3.000000000000000000 ) ;
#9163 = ORIENTED_EDGE ( 'NONE', *, *, #18652, .T. ) ;
#9164 = AXIS2_PLACEMENT_3D ( 'NONE', #2222, #20107, #7408 ) ;
#9165 = AXIS2_PLACEMENT_3D ( 'NONE', #315, #2416, #9252 ) ;
#9166 = AXIS2_PLACEMENT_3D ( 'NONE', #14337, #12573, #19757 ) ;
#9167 = DIRECTION ( 'NONE',  ( 0.6819983600624971443, -0.7313537016191717921, 0.000000000000000000 ) ) ;
#9168 = ORIENTED_EDGE ( 'NONE', *, *, #10839, .F. ) ;
#9169 = PLANE ( 'NONE',  #3162 ) ;
#9170 = DIRECTION ( 'NONE',  ( -0.000000000000000000, 1.000000000000000000, -0.000000000000000000 ) ) ;
#9171 = CARTESIAN_POINT ( 'NONE',  ( 25.60000000000000142, 0.000000000000000000, -6.938893903907228378E-15 ) ) ;
#9172 = VERTEX_POINT ( 'NONE', #3183 ) ;
#9173 = CARTESIAN_POINT ( 'NONE',  ( 4.050480423730732582, -1.376911654797400075, 3.567926555162021174 ) ) ;
#9174 = CARTESIAN_POINT ( 'NONE',  ( 1.030796516412017860, 0.6000000000000129674, -4.508445023301312027 ) ) ;
#9175 = DIRECTION ( 'NONE',  ( -1.000000000000000000, 4.190823558986610327E-31, -1.733449886265890494E-32 ) ) ;
#9176 = CARTESIAN_POINT ( 'NONE',  ( 7.554637128289433790, -13.87985946887537558, 7.453047528892627227 ) ) ;
#9177 = CARTESIAN_POINT ( 'NONE',  ( 8.178874953434442929, -13.99214848402183797, 6.644730819939103306 ) ) ;
#9178 = CARTESIAN_POINT ( 'NONE',  ( -12.84999999999999964, -14.00000000000003020, 5.750000000000032863 ) ) ;
#9179 = CONICAL_SURFACE ( 'NONE', #9545, 3.499999999999999556, 1.047197551196600074 ) ;
#9180 = DIRECTION ( 'NONE',  ( 0.000000000000000000, 0.000000000000000000, -1.000000000000000000 ) ) ;
#9181 = DIRECTION ( 'NONE',  ( -3.330669073875432643E-16, -4.437342591868153746E-31, 1.000000000000000000 ) ) ;
#9182 = SURFACE_STYLE_USAGE ( .BOTH. , #1990 ) ;
#9183 = CARTESIAN_POINT ( 'NONE',  ( 3.999999999999939160, 0.9868501483902684113, -0.09357334158575086880 ) ) ;
#9184 = APPLICATION_PROTOCOL_DEFINITION ( 'draft international standard', 'automotive_design', 1998, #15945 ) ;
#9186 = ORIENTED_EDGE ( 'NONE', *, *, #18748, .T. ) ;
#9185 = ORIENTED_EDGE ( 'NONE', *, *, #20527, .F. ) ;
#9187 = EDGE_CURVE ( 'NONE', #20539, #9220, #7064, .T. ) ;
#9188 = EDGE_LOOP ( 'NONE', ( #17158, #6640, #8266, #18048 ) ) ;
#9189 = CIRCLE ( 'NONE', #22348, 5.500000000000033751 ) ;
#9191 = ORIENTED_EDGE ( 'NONE', *, *, #3528, .T. ) ;
#9190 = ORIENTED_EDGE ( 'NONE', *, *, #16456, .F. ) ;
#9192 = B_SPLINE_CURVE_WITH_KNOTS ( 'NONE', 3,
 ( #20504, #8257, #16936, #13197 ),
 .UNSPECIFIED., .F., .F.,
 ( 4, 4 ),
 ( 2.380739282289325661E-07, 0.002044882221487581784 ),
 .UNSPECIFIED. ) ;
#9193 = VECTOR ( 'NONE', #6274, 999.9999999999998863 ) ;
#9194 = FACE_OUTER_BOUND ( 'NONE', #1031, .T. ) ;
#9195 = CARTESIAN_POINT ( 'NONE',  ( 37.54332536350039362, 0.1155932590976206792, -2.779374676783886056 ) ) ;
#9196 = CARTESIAN_POINT ( 'NONE',  ( 8.954763739086837759, -12.50000000000004619, 6.678571428571492774 ) ) ;
#9197 = CARTESIAN_POINT ( 'NONE',  ( 0.000000000000000000, -1.750000000000001554, 0.000000000000000000 ) ) ;
#9198 = CARTESIAN_POINT ( 'NONE',  ( -4.550510256924974684, 35.99999999900384751, -25.50000000000000000 ) ) ;
#9199 = CARTESIAN_POINT ( 'NONE',  ( 4.175572532730925879, -2.061029303918044064, 3.569807470274392269 ) ) ;
#9200 = DIRECTION ( 'NONE',  ( 0.000000000000000000, 0.000000000000000000, 1.000000000000000000 ) ) ;
#9201 = LINE ( 'NONE', #5093, #6177 ) ;
#9202 = CARTESIAN_POINT ( 'NONE',  ( -95.70000000000069917, 0.5000000000000073275, 8.000000000000090594 ) ) ;
#9203 = DIRECTION ( 'NONE',  ( -7.860214984770699307E-18, 1.409037165336591006E-16, 1.000000000000000000 ) ) ;
#9204 = DIRECTION ( 'NONE',  ( -0.5150787536377134934, 0.000000000000000000, 0.8571428571428567622 ) ) ;
#9205 = B_SPLINE_CURVE_WITH_KNOTS ( 'NONE', 3,
 ( #12780, #20432, #2304, #18542 ),
 .UNSPECIFIED., .F., .F.,
 ( 4, 4 ),
 ( 0.004330357959029864159, 0.008660484977952059155 ),
 .UNSPECIFIED. ) ;
#9206 = CARTESIAN_POINT ( 'NONE',  ( -56.54644007500109382, -0.5000000000001045830, -8.666666666666655416 ) ) ;
#9207 = DIRECTION ( 'NONE',  ( 0.000000000000000000, -7.888609052210126812E-31, 1.000000000000000000 ) ) ;
#9208 = CIRCLE ( 'NONE', #22360, 7.499999999999998224 ) ;
#9209 = AXIS2_PLACEMENT_3D ( 'NONE', #15657, #16007, #5318 ) ;
#9210 = DIRECTION ( 'NONE',  ( -2.220446049250313081E-16, 1.000000000000000000, -7.025792437124636392E-31 ) ) ;
#9211 = CARTESIAN_POINT ( 'NONE',  ( -4.990285246490005377, 35.99999999900386172, -19.46466550946063023 ) ) ;
#9212 = CARTESIAN_POINT ( 'NONE',  ( 8.954763739086837759, -0.4999999999999852895, 6.678571428571446589 ) ) ;
#9213 = ORIENTED_EDGE ( 'NONE', *, *, #2640, .T. ) ;
#9214 =( LENGTH_UNIT ( ) NAMED_UNIT ( * ) SI_UNIT ( .MILLI., .METRE. ) );
#9216 = EDGE_LOOP ( 'NONE', ( #13444, #10197, #19422 ) ) ;
#9215 = ORIENTED_EDGE ( 'NONE', *, *, #8668, .T. ) ;
#9217 = ADVANCED_FACE ( 'NONE', ( #23181 ), #17951, .F. ) ;
#9218 = VERTEX_POINT ( 'NONE', #6946 ) ;
#9220 = VERTEX_POINT ( 'NONE', #6819 ) ;
#9219 = EDGE_LOOP ( 'NONE', ( #14535, #3150 ) ) ;
#9221 = ORIENTED_EDGE ( 'NONE', *, *, #15423, .T. ) ;
#9222 = FACE_OUTER_BOUND ( 'NONE', #10289, .T. ) ;
#9223 = ORIENTED_EDGE ( 'NONE', *, *, #21666, .T. ) ;
#9224 = VERTEX_POINT ( 'NONE', #5289 ) ;
#9225 = DIRECTION ( 'NONE',  ( -1.000000000000000000, -1.479114197289397135E-31, -5.916456789157588541E-31 ) ) ;
#9226 = EDGE_CURVE ( 'NONE', #8320, #15636, #13988, .T. ) ;
#9227 = AXIS2_PLACEMENT_3D ( 'NONE', #1076, #18706, #18946 ) ;
#9228 = EDGE_CURVE ( 'NONE', #2293, #2880, #4638, .T. ) ;
#9229 = DIRECTION ( 'NONE',  ( -1.000000000000000000, -2.699383410053119293E-30, -4.336808689941968432E-16 ) ) ;
#9230 = EDGE_CURVE ( 'NONE', #2822, #9536, #7648, .T. ) ;
#9231 = DIRECTION ( 'NONE',  ( -1.000000000000000000, 0.000000000000000000, 0.000000000000000000 ) ) ;
#9232 = CARTESIAN_POINT ( 'NONE',  ( 4.132952817037863547, -2.031684012687315466, -3.518979934899742812 ) ) ;
#9233 = LINE ( 'NONE', #3931, #6704 ) ;
#9234 = DIRECTION ( 'NONE',  ( -0.000000000000000000, -1.000000000000000000, -0.000000000000000000 ) ) ;
#9235 = FACE_OUTER_BOUND ( 'NONE', #2528, .T. ) ;
#9236 = DIRECTION ( 'NONE',  ( -0.000000000000000000, 1.000000000000000000, 0.000000000000000000 ) ) ;
#9237 = DIRECTION ( 'NONE',  ( -1.000000000000000000, -2.699383410053120695E-30, -3.885780586188017323E-16 ) ) ;
#9238 = CARTESIAN_POINT ( 'NONE',  ( 37.42127086598728170, 10.78233971064650731, -2.578729134013173940 ) ) ;
#9239 = ORIENTED_EDGE ( 'NONE', *, *, #13750, .T. ) ;
#9240 = EDGE_CURVE ( 'NONE', #9100, #1329, #5778, .T. ) ;
#9241 = FILL_AREA_STYLE_COLOUR ( '', #16856 ) ;
#9242 = DIRECTION ( 'NONE',  ( 1.000000000000000000, 2.699383410053119644E-30, 3.330669073875432643E-16 ) ) ;
#9244 = ORIENTED_EDGE ( 'NONE', *, *, #16023, .F. ) ;
#9243 = ORIENTED_EDGE ( 'NONE', *, *, #21410, .T. ) ;
#9245 = ORIENTED_EDGE ( 'NONE', *, *, #12707, .F. ) ;
#9246 = VECTOR ( 'NONE', #22742, 1000.000000000000000 ) ;
#9247 = ORIENTED_EDGE ( 'NONE', *, *, #14867, .T. ) ;
#9249 = ORIENTED_EDGE ( 'NONE', *, *, #4183, .F. ) ;
#9248 = EDGE_CURVE ( 'NONE', #1201, #8077, #12908, .T. ) ;
#9250 = ADVANCED_FACE ( 'NONE', ( #12090 ), #21531, .F. ) ;
#9251 = COLOUR_RGB ( '', 0.08235294, 0.09019608, 0.10196078) ;
#9252 = DIRECTION ( 'NONE',  ( -0.6819983600625070252, -0.7313537016191624662, 0.000000000000000000 ) ) ;
#9253 = EDGE_CURVE ( 'NONE', #13233, #3913, #15829, .T. ) ;
#9254 = DIRECTION ( 'NONE',  ( -2.013525853228507892E-32, -6.902532920683810383E-31, 1.000000000000000000 ) ) ;
#9255 = ADVANCED_FACE ( 'NONE', ( #1526 ), #18925, .T. ) ;
#9256 = CARTESIAN_POINT ( 'NONE',  ( 4.114405500665259119, -2.025575754679715068, -3.508400121684936313 ) ) ;
#9257 = DIRECTION ( 'NONE',  ( -1.000000000000000000, -8.030776666391858360E-17, -3.330669073875458281E-16 ) ) ;
#9258 = AXIS2_PLACEMENT_3D ( 'NONE', #21738, #12663, #10676 ) ;
#9259 = DIRECTION ( 'NONE',  ( 0.5833333333333320381, 1.429810390713075314E-30, -0.8122328620674146293 ) ) ;
#9260 = DIRECTION ( 'NONE',  ( 0.000000000000000000, 0.000000000000000000, -1.000000000000000000 ) ) ;
#9261 = DIRECTION ( 'NONE',  ( 1.550910762415566494E-16, 1.000000000000000000, -8.135128085091684243E-31 ) ) ;
#9262 =( BOUNDED_SURFACE ( )  B_SPLINE_SURFACE ( 3, 2, ( 
 ( #21712, #10758, #9007 ),
 ( #12760, #16278, #16159 ),
 ( #14642, #18066, #77 ),
 ( #7140, #7247, #19823 ),
 ( #19945, #12637, #21603 ),
 ( #11103, #5249, #8887 ) ),
 .UNSPECIFIED., .F., .F., .F. ) 
 B_SPLINE_SURFACE_WITH_KNOTS ( ( 4, 2, 4 ),
 ( 3, 3 ),
 ( 0.02032853247518129000, 0.02278863295364823988, 0.02524873343211518975 ),
 ( 0.000000000000000000, 1.000000000000000000 ),
 .UNSPECIFIED. ) 
 GEOMETRIC_REPRESENTATION_ITEM ( )  RATIONAL_B_SPLINE_SURFACE ( (
 ( 1.000000000000000000, 0.8047781615896834051, 1.000000000000000000),
 ( 1.000000000000000000, 0.8123767586289972753, 1.000000000000000000),
 ( 1.000000000000000000, 0.8190662415563431109, 1.000000000000000000),
 ( 1.000000000000000000, 0.8192361015669969992, 1.000000000000000000),
 ( 1.000000000000000000, 0.8126135807103180841, 1.000000000000000000),
 ( 1.000000000000000000, 0.8047712338318581127, 1.000000000000000000) ) ) 
 REPRESENTATION_ITEM ( '' )  SURFACE ( )  );
#9263 = CARTESIAN_POINT ( 'NONE',  ( -7.000000000000020428, -3.018576030000264865, 8.916666666666712260 ) ) ;
#9264 = DIRECTION ( 'NONE',  ( 2.013525853228507892E-32, 6.902532920683810383E-31, -1.000000000000000000 ) ) ;
#9265 = LINE ( 'NONE', #13146, #16660 ) ;
#9266 = DIRECTION ( 'NONE',  ( -1.000000000000000000, 0.000000000000000000, -4.336808689941968432E-16 ) ) ;
#9267 = DIRECTION ( 'NONE',  ( 1.000000000000000000, -1.550910762415513985E-16, -3.012982189080959477E-32 ) ) ;
#9268 = VECTOR ( 'NONE', #19829, 1000.000000000000114 ) ;
#9269 = EDGE_CURVE ( 'NONE', #19664, #5108, #1639, .T. ) ;
#9270 = CARTESIAN_POINT ( 'NONE',  ( -43.10883117545713361, 4.565685424949256443, 8.000000000000035527 ) ) ;
#9271 = DIRECTION ( 'NONE',  ( 0.000000000000000000, 0.000000000000000000, 1.000000000000000000 ) ) ;
#9272 = ORIENTED_EDGE ( 'NONE', *, *, #21914, .F. ) ;
#9273 = ORIENTED_EDGE ( 'NONE', *, *, #14656, .T. ) ;
#9274 = ADVANCED_FACE ( 'NONE', ( #696 ), #7629, .F. ) ;
#9275 = CARTESIAN_POINT ( 'NONE',  ( -6.000000000000088818, -2.000000000000043521, 7.500000000000076383 ) ) ;
#9276 = CARTESIAN_POINT ( 'NONE',  ( 0.2499999999999724665, 0.2500000000000140998, 0.000000000000000000 ) ) ;
#9277 = ORIENTED_EDGE ( 'NONE', *, *, #19319, .F. ) ;
#9278 = CARTESIAN_POINT ( 'NONE',  ( -4.950765356264097861, 36.36782871084110980, -18.97560888259267387 ) ) ;
#9279 = DIRECTION ( 'NONE',  ( 1.000000000000000000, 4.252453317207022018E-31, -5.551115123125818447E-17 ) ) ;
#9280 = CARTESIAN_POINT ( 'NONE',  ( 3.878096787214585284, -3.381939201670153938, -1.142309474598458774 ) ) ;
#9281 = CIRCLE ( 'NONE', #15276, 2.550000000000003819 ) ;
#9282 = CARTESIAN_POINT ( 'NONE',  ( -6.938893903907228378E-15, -22.91099746826335348, -1.387778780781445676E-14 ) ) ;
#9283 = FACE_OUTER_BOUND ( 'NONE', #16970, .T. ) ;
#9284 = COLOUR_RGB ( '', 0.66274510, 0.83137255, 0.94901961) ;
#9285 = CARTESIAN_POINT ( 'NONE',  ( 5.599999999999995204, 7.939204849094524965E-15, 2.500000000000001332 ) ) ;
#9286 = CARTESIAN_POINT ( 'NONE',  ( 0.000000000000000000, 0.000000000000000000, -5.600000000000000533 ) ) ;
#9287 = CIRCLE ( 'NONE', #2136, 2.550000000000000266 ) ;
#9288 = FACE_OUTER_BOUND ( 'NONE', #12185, .T. ) ;
#9289 = DIRECTION ( 'NONE',  ( 0.000000000000000000, -1.000000000000000000, 0.000000000000000000 ) ) ;
#9290 = DIRECTION ( 'NONE',  ( -8.438582421954109416E-32, 0.000000000000000000, -1.000000000000000000 ) ) ;
#9291 = CIRCLE ( 'NONE', #12278, 0.4999999999999995559 ) ;
#9292 = CARTESIAN_POINT ( 'NONE',  ( 30.00000000029184832, -9.961476088449217059E-10, -41.54999999999999716 ) ) ;
#9293 = DIRECTION ( 'NONE',  ( -0.7313537016191733464, 0.6819983600624954789, -3.733258675956565293E-18 ) ) ;
#9294 = DIRECTION ( 'NONE',  ( 3.241725282392603095E-30, 1.000000000000000000, -2.218671295934100958E-31 ) ) ;
#9295 =( NAMED_UNIT ( * ) PLANE_ANGLE_UNIT ( ) SI_UNIT ( $, .RADIAN. ) );
#9296 = CARTESIAN_POINT ( 'NONE',  ( 3.880206590543185730, -2.665671387532593251, -2.382921720510934094 ) ) ;
#9297 = VECTOR ( 'NONE', #14904, 1000.000000000000114 ) ;
#9298 = APPLICATION_PROTOCOL_DEFINITION ( 'draft international standard', 'automotive_design', 1998, #15079 ) ;
#9299 = VERTEX_POINT ( 'NONE', #4092 ) ;
#9300 = AXIS2_PLACEMENT_3D ( 'NONE', #4320, #9408, #16782 ) ;
#9301 = EDGE_CURVE ( 'NONE', #6421, #18645, #16649, .T. ) ;
#9302 = VERTEX_POINT ( 'NONE', #14568 ) ;
#9303 = AXIS2_PLACEMENT_3D ( 'NONE', #9439, #7784, #848 ) ;
#9305 = ORIENTED_EDGE ( 'NONE', *, *, #20882, .F. ) ;
#9304 = EDGE_LOOP ( 'NONE', ( #23016, #23094, #9273, #20275 ) ) ;
#9306 = DIRECTION ( 'NONE',  ( -2.013525853228507892E-32, -6.902532920683810383E-31, 1.000000000000000000 ) ) ;
#9307 = EDGE_CURVE ( 'NONE', #14358, #14050, #20225, .T. ) ;
#9308 = CARTESIAN_POINT ( 'NONE',  ( 37.34641016151396542, 0.3999999999999052647, -2.653589838486210883 ) ) ;
#9309 = CARTESIAN_POINT ( 'NONE',  ( 7.500000000000007994, -11.57130297832598309, 9.041853041260921486 ) ) ;
#9310 = DIRECTION ( 'NONE',  ( -4.019602852144215652E-47, -6.982962677686261977E-15, -1.000000000000000000 ) ) ;
#9311 = CIRCLE ( 'NONE', #4048, 4.000000000000023981 ) ;
#9312 = DIRECTION ( 'NONE',  ( 1.000000000000000000, -4.615739097524200579E-16, -1.134196829589820086E-15 ) ) ;
#9313 = PLANE ( 'NONE',  #867 ) ;
#9314 = AXIS2_PLACEMENT_3D ( 'NONE', #4388, #4515, #15090 ) ;
#9315 = CARTESIAN_POINT ( 'NONE',  ( -5.403531933167068146, 36.45753077221091587, -16.34652230730261380 ) ) ;
#9316 = FILL_AREA_STYLE ('',( #18605 ) ) ;
#9317 = DIRECTION ( 'NONE',  ( 1.107262168541282614E-16, -1.107262168541365321E-16, 1.000000000000000000 ) ) ;
#9318 = DIRECTION ( 'NONE',  ( 1.000000000000000000, 0.000000000000000000, 0.000000000000000000 ) ) ;
#9319 = DIRECTION ( 'NONE',  ( 1.000000000000000000, -4.190823558986610327E-31, 1.733449886265890494E-32 ) ) ;
#9320 = AXIS2_PLACEMENT_3D ( 'NONE', #14320, #8677, #5394 ) ;
#9321 = DIRECTION ( 'NONE',  ( 1.000000000000000000, -5.773159728050815588E-15, 0.000000000000000000 ) ) ;
#9322 = CARTESIAN_POINT ( 'NONE',  ( 30.00000000029184832, 2.999999999003851503, -39.00000000000000000 ) ) ;
#9323 = FACE_OUTER_BOUND ( 'NONE', #14073, .T. ) ;
#9324 = VECTOR ( 'NONE', #4591, 1000.000000000000000 ) ;
#9325 = VECTOR ( 'NONE', #4104, 1000.000000000000000 ) ;
#9326 = DIRECTION ( 'NONE',  ( -0.6819983600624940356, 0.7313537016191746787, 1.110361430785838977E-16 ) ) ;
#9327 = AXIS2_PLACEMENT_3D ( 'NONE', #17231, #9837, #18778 ) ;
#9328 = LINE ( 'NONE', #4018, #9683 ) ;
#9329 = CARTESIAN_POINT ( 'NONE',  ( 8.115139842999449016, -0.1079360712687435775, 7.423524081915865658 ) ) ;
#9330 = ORIENTED_EDGE ( 'NONE', *, *, #7092, .F. ) ;
#9332 = VERTEX_POINT ( 'NONE', #7401 ) ;
#9331 = ORIENTED_EDGE ( 'NONE', *, *, #17269, .T. ) ;
#9333 = AXIS2_PLACEMENT_3D ( 'NONE', #11426, #6489, #20856 ) ;
#9334 = VERTEX_POINT ( 'NONE', #20101 ) ;
#9336 = ORIENTED_EDGE ( 'NONE', *, *, #16840, .T. ) ;
#9335 = EDGE_LOOP ( 'NONE', ( #22211, #1610, #16399, #2464 ) ) ;
#9337 = ORIENTED_EDGE ( 'NONE', *, *, #23179, .T. ) ;
#9338 = CARTESIAN_POINT ( 'NONE',  ( -4.578118944855300576, -1.701165921963301964, 1.570465384416986021 ) ) ;
#9339 = ORIENTED_EDGE ( 'NONE', *, *, #21155, .F. ) ;
#9340 = ORIENTED_EDGE ( 'NONE', *, *, #16103, .F. ) ;
#9341 = CARTESIAN_POINT ( 'NONE',  ( 0.4436723136282449964, 0.6000000000000134115, 4.148801034132779897 ) ) ;
#9342 = AXIS2_PLACEMENT_3D ( 'NONE', #21411, #17624, #3732 ) ;
#9343 = VECTOR ( 'NONE', #220, 1000.000000000000000 ) ;
#9344 = AXIS2_PLACEMENT_3D ( 'NONE', #2889, #22312, #20899 ) ;
#9345 = DIRECTION ( 'NONE',  ( 1.000000000000000000, -4.440892098500650814E-16, -7.860214984771115307E-18 ) ) ;
#9346 = CARTESIAN_POINT ( 'NONE',  ( 58.85734743794747459, 0.7537990605245292741, 6.000000000000158096 ) ) ;
#9347 = CARTESIAN_POINT ( 'NONE',  ( -7.670621117724356175, -2.511599330828965027, 8.215271161873788586 ) ) ;
#9348 = PRODUCT_DEFINITION ( 'UNKNOWN', '', #3744, #4630 ) ;
#9349 = CARTESIAN_POINT ( 'NONE',  ( 0.2174200650117729394, 2.185595227304866661, -3.214438021527967759 ) ) ;
#9350 = CARTESIAN_POINT ( 'NONE',  ( 3.951447005078455366, -3.704664227300149548, -0.5833333333333268200 ) ) ;
#9351 = CARTESIAN_POINT ( 'NONE',  ( 110.9706201109471522, -9.453020409440265226, 6.500000000000095923 ) ) ;
#9352 = DIRECTION ( 'NONE',  ( 0.2405376366294550983, 0.000000000000000000, -0.9706398123736303951 ) ) ;
#9353 = COLOUR_RGB ( '', 0.31764706, 0.68627451, 0.89019608) ;
#9354 = EDGE_CURVE ( 'NONE', #12275, #10139, #13161, .T. ) ;
#9355 = DIRECTION ( 'NONE',  ( 1.000000000000000000, -8.030776666391948340E-17, 3.330669073875457788E-16 ) ) ;
#9356 = AXIS2_PLACEMENT_3D ( 'NONE', #13537, #8125, #20951 ) ;
#9357 = CARTESIAN_POINT ( 'NONE',  ( 37.86602540378461157, 11.00000000000000533, -2.133974596215514552 ) ) ;
#9358 = ORIENTED_EDGE ( 'NONE', *, *, #348, .T. ) ;
#9359 = CONICAL_SURFACE ( 'NONE', #22511, 4.000000000000022204, 0.8911886515913840512 ) ;
#9360 = EDGE_CURVE ( 'NONE', #2500, #20007, #7292, .T. ) ;
#9361 = VECTOR ( 'NONE', #13492, 1000.000000000000000 ) ;
#9362 = CYLINDRICAL_SURFACE ( 'NONE', #21776, 6.500000000000052403 ) ;
#9364 = ORIENTED_EDGE ( 'NONE', *, *, #10964, .T. ) ;
#9363 = ORIENTED_EDGE ( 'NONE', *, *, #6808, .T. ) ;
#9365 = ORIENTED_EDGE ( 'NONE', *, *, #14163, .T. ) ;
#9366 = ORIENTED_EDGE ( 'NONE', *, *, #11370, .T. ) ;
#9367 = EDGE_LOOP ( 'NONE', ( #20359, #12261, #16827 ) ) ;
#9368 = VERTEX_POINT ( 'NONE', #7516 ) ;
#9369 = ORIENTED_EDGE ( 'NONE', *, *, #6231, .T. ) ;
#9370 = VERTEX_POINT ( 'NONE', #3741 ) ;
#9371 = DIRECTION ( 'NONE',  ( 1.000000000000000000, 2.699383410053119644E-30, 3.330669073875432643E-16 ) ) ;
#9372 = CARTESIAN_POINT ( 'NONE',  ( 2.775557561562891351E-14, 11.00000000000000000, -6.499999999999950262 ) ) ;
#9373 = DIRECTION ( 'NONE',  ( -4.003208021484906984E-16, 0.000000000000000000, 1.000000000000000000 ) ) ;
#9374 = EDGE_CURVE ( 'NONE', #21109, #280, #15533, .T. ) ;
#9375 = CIRCLE ( 'NONE', #10493, 2.499999999999993783 ) ;
#9376 = CARTESIAN_POINT ( 'NONE',  ( -0.6448876103709475505, -4.246476118072399331, -0.2256878752777136121 ) ) ;
#9377 = DIRECTION ( 'NONE',  ( 0.7071067811865535679, -0.7071067811865414665, 0.000000000000000000 ) ) ;
#9378 = LINE ( 'NONE', #4536, #14701 ) ;
#9379 = CARTESIAN_POINT ( 'NONE',  ( 0.000000000000000000, 0.000000000000000000, 0.000000000000000000 ) ) ;
#9380 = ADVANCED_FACE ( 'NONE', ( #7862 ), #9169, .T. ) ;
#9381 = DIRECTION ( 'NONE',  ( -0.6819983600625060260, -0.7313537016191635765, -6.106365041599011361E-16 ) ) ;
#9382 = DIRECTION ( 'NONE',  ( -0.000000000000000000, 1.000000000000000000, 0.000000000000000000 ) ) ;
#9383 = CARTESIAN_POINT ( 'NONE',  ( 1.200000000000006617, -0.5999999999999894307, -4.749999999999948486 ) ) ;
#9384 = DIRECTION ( 'NONE',  ( 3.032184104443272185E-30, 1.000000000000000000, -7.395570986447005381E-32 ) ) ;
#9385 = AXIS2_PLACEMENT_3D ( 'NONE', #5195, #3319, #13897 ) ;
#9386 = EDGE_CURVE ( 'NONE', #4546, #2242, #21570, .T. ) ;
#9387 = SURFACE_STYLE_FILL_AREA ( #797 ) ;
#9388 = PLANE ( 'NONE',  #8579 ) ;
#9389 = LINE ( 'NONE', #11481, #9297 ) ;
#9390 = EDGE_CURVE ( 'NONE', #13703, #18075, #2615, .T. ) ;
#9391 = EDGE_CURVE ( 'NONE', #20161, #21498, #1281, .T. ) ;
#9392 = B_SPLINE_CURVE_WITH_KNOTS ( 'NONE', 3,
 ( #8673, #10667, #15027, #21396, #19495, #22797, #12545, #3391, #13958, #17969, #16065, #5022, #14208, #15830 ),
 .UNSPECIFIED., .F., .F.,
 ( 4, 2, 2, 2, 2, 2, 4 ),
 ( 0.000000000000000000, 0.0008249779604813560832, 0.001237466940722032173, 0.001649955920962708480, 0.002062444901203385871, 0.002474933881444063913, 0.003299911841925418261 ),
 .UNSPECIFIED. ) ;
#9393 = ORIENTED_EDGE ( 'NONE', *, *, #7649, .T. ) ;
#9394 = LINE ( 'NONE', #21981, #15500 ) ;
#9395 = CARTESIAN_POINT ( 'NONE',  ( -4.000000000000087041, 2.309401076758546445, -5.000000000000000888 ) ) ;
#9396 = ORIENTED_EDGE ( 'NONE', *, *, #3592, .T. ) ;
#9397 = VECTOR ( 'NONE', #10978, 1000.000000000000000 ) ;
#9398 = CARTESIAN_POINT ( 'NONE',  ( -4.751720029897056996, 36.43339712399806274, -19.00000000000001066 ) ) ;
#9399 = DIRECTION ( 'NONE',  ( -1.000000000000000000, 4.437342591868175641E-31, -3.330669073875457788E-16 ) ) ;
#9400 = ADVANCED_FACE ( 'NONE', ( #2446 ), #22098, .T. ) ;
#9401 = DIRECTION ( 'NONE',  ( 0.000000000000000000, 0.000000000000000000, 1.000000000000000000 ) ) ;
#9402 = CARTESIAN_POINT ( 'NONE',  ( 4.055492966679538291, -2.385006769472565402, -3.005124364834383943 ) ) ;
#9403 = CARTESIAN_POINT ( 'NONE',  ( 108.2426266706971205, -10.52760560296367487, -6.500000000000075495 ) ) ;
#9404 = FACE_OUTER_BOUND ( 'NONE', #15630, .T. ) ;
#9405 = EDGE_CURVE ( 'NONE', #4871, #8586, #3236, .T. ) ;
#9406 = EDGE_CURVE ( 'NONE', #18021, #16591, #20376, .T. ) ;
#9407 = CARTESIAN_POINT ( 'NONE',  ( 24.75000000000001066, 2.000000000000099032, -16.99999999999997868 ) ) ;
#9408 = DIRECTION ( 'NONE',  ( -0.000000000000000000, -0.000000000000000000, 1.000000000000000000 ) ) ;
#9409 = CARTESIAN_POINT ( 'NONE',  ( 35.50000000029184832, 2.999999999003851503, -26.50000000000000000 ) ) ;
#9410 = LINE ( 'NONE', #16554, #17794 ) ;
#9411 = CARTESIAN_POINT ( 'NONE',  ( 7.694134585029463125, -13.68800912542550741, 8.172315317061212170 ) ) ;
#9412 = CARTESIAN_POINT ( 'NONE',  ( 2.775557561562891351E-14, 0.2500000000000106581, -10.43301270189220276 ) ) ;
#9413 = DIRECTION ( 'NONE',  ( -1.000000000000000000, 0.000000000000000000, 0.000000000000000000 ) ) ;
#9414 = DIRECTION ( 'NONE',  ( -0.7313537016191746787, -0.6819983600624941467, -1.072890437865584409E-16 ) ) ;
#9415 = EDGE_CURVE ( 'NONE', #343, #3554, #21865, .T. ) ;
#9416 = DIRECTION ( 'NONE',  ( -1.000000000000000000, -1.910522504832140594E-31, 5.551115123125818447E-17 ) ) ;
#9417 = ADVANCED_FACE ( 'NONE', ( #15253 ), #10094, .T. ) ;
#9418 = CARTESIAN_POINT ( 'NONE',  ( 3.948103430090708521, -3.379418997638742539, -1.146674596026139303 ) ) ;
#9419 = CIRCLE ( 'NONE', #15777, 2.550000000000012701 ) ;
#9420 = APPLICATION_PROTOCOL_DEFINITION ( 'draft international standard', 'automotive_design', 1998, #1425 ) ;
#9421 = VERTEX_POINT ( 'NONE', #18675 ) ;
#9423 = VERTEX_POINT ( 'NONE', #11493 ) ;
#9422 = ORIENTED_EDGE ( 'NONE', *, *, #10091, .T. ) ;
#9424 = DIRECTION ( 'NONE',  ( 1.000000000000000000, -5.551115122690158919E-17, 1.001543064812511222E-16 ) ) ;
#9425 = CARTESIAN_POINT ( 'NONE',  ( 37.86602540378471815, -1.973247953923618070E-14, -2.133974596215504338 ) ) ;
#9426 = DIRECTION ( 'NONE',  ( -1.000000000000000000, -2.699383410053119644E-30, -3.330669073875432643E-16 ) ) ;
#9427 = ORIENTED_EDGE ( 'NONE', *, *, #21471, .F. ) ;
#9428 = VECTOR ( 'NONE', #13538, 1000.000000000000000 ) ;
#9429 = CARTESIAN_POINT ( 'NONE',  ( -6.000000000000074607, 1.999999999999960032, 7.500000000000062172 ) ) ;
#9430 = CARTESIAN_POINT ( 'NONE',  ( 1.318389841742373392E-16, -14.99999999999997691, 4.749999999999999112 ) ) ;
#9431 = DIRECTION ( 'NONE',  ( 1.000000000000000000, 4.252453317207022018E-31, -5.551115123125818447E-17 ) ) ;
#9432 = CARTESIAN_POINT ( 'NONE',  ( 1.199999999999992628, -0.5999999999999963141, 4.543283425070391068 ) ) ;
#9433 = DIRECTION ( 'NONE',  ( -7.395570986446975166E-31, -3.382522293539642681E-32, -1.000000000000000000 ) ) ;
#9434 = CARTESIAN_POINT ( 'NONE',  ( 0.000000000000000000, 0.000000000000000000, -0.2800830152838856835 ) ) ;
#9435 = DIRECTION ( 'NONE',  ( 0.000000000000000000, 0.000000000000000000, -1.000000000000000000 ) ) ;
#9436 = CARTESIAN_POINT ( 'NONE',  ( -12.85000000000002807, -1.999999999999998224, 6.249999999999950262 ) ) ;
#9437 = SURFACE_SIDE_STYLE ('',( #4352 ) ) ;
#9438 = CARTESIAN_POINT ( 'NONE',  ( -3.999999999708153453, 38.99999999900385461, -26.50000000000000000 ) ) ;
#9439 = CARTESIAN_POINT ( 'NONE',  ( 6.999999999999992006, -8.000000000000051514, 6.249999999999977796 ) ) ;
#9440 = CARTESIAN_POINT ( 'NONE',  ( -6.000000000000074607, 4.799999999999964295, 7.500000000000062172 ) ) ;
#9441 = CARTESIAN_POINT ( 'NONE',  ( 7.876571740167059410, -0.1939399797844648943, 7.785394814390983242 ) ) ;
#9442 = ADVANCED_FACE ( 'NONE', ( #22336 ), #20004, .T. ) ;
#9443 = ORIENTED_EDGE ( 'NONE', *, *, #4907, .T. ) ;
#9444 = CIRCLE ( 'NONE', #15444, 3.500000000000023981 ) ;
#9445 = VECTOR ( 'NONE', #7672, 1000.000000000000000 ) ;
#9447 = VERTEX_POINT ( 'NONE', #18920 ) ;
#9446 = VERTEX_POINT ( 'NONE', #2562 ) ;
#9448 = ORIENTED_EDGE ( 'NONE', *, *, #20032, .T. ) ;
#9449 = ORIENTED_EDGE ( 'NONE', *, *, #12716, .T. ) ;
#9451 = VERTEX_POINT ( 'NONE', #10198 ) ;
#9450 = ORIENTED_EDGE ( 'NONE', *, *, #22711, .T. ) ;
#9452 = VERTEX_POINT ( 'NONE', #8214 ) ;
#9453 = LINE ( 'NONE', #4370, #7616 ) ;
#9454 = B_SPLINE_CURVE_WITH_KNOTS ( 'NONE', 3,
 ( #2205, #13260, #20443, #5865, #5631, #5979 ),
 .UNSPECIFIED., .F., .F.,
 ( 4, 2, 4 ),
 ( 0.002336974151641598059, 0.003500975885716476645, 0.004664977619791355230 ),
 .UNSPECIFIED. ) ;
#9455 = ORIENTED_EDGE ( 'NONE', *, *, #9638, .F. ) ;
#9456 = ORIENTED_EDGE ( 'NONE', *, *, #23030, .T. ) ;
#9457 = DIRECTION ( 'NONE',  ( -1.000000000000000000, 0.000000000000000000, 0.000000000000000000 ) ) ;
#9458 = DIRECTION ( 'NONE',  ( -1.000000000000000000, 4.440892098500641939E-16, 0.000000000000000000 ) ) ;
#9459 = DIRECTION ( 'NONE',  ( 3.032184104443272185E-30, 1.000000000000000000, -7.395570986447005381E-32 ) ) ;
#9460 = DIRECTION ( 'NONE',  ( -2.013525853228507892E-32, -6.902532920683810383E-31, 1.000000000000000000 ) ) ;
#9461 = CARTESIAN_POINT ( 'NONE',  ( 63.53596085922838199, -2.925414806476733798, -6.000000000000060396 ) ) ;
#9462 = DIRECTION ( 'NONE',  ( 0.000000000000000000, 0.000000000000000000, -1.000000000000000000 ) ) ;
#9463 = AXIS2_PLACEMENT_3D ( 'NONE', #7398, #22095, #19869 ) ;
#9464 = DIRECTION ( 'NONE',  ( 5.551115123125733398E-17, 0.000000000000000000, -1.000000000000000000 ) ) ;
#9465 = CARTESIAN_POINT ( 'NONE',  ( 37.86602540378459025, -1.387778780781445676E-14, -2.133974596215476360 ) ) ;
#9466 = CARTESIAN_POINT ( 'NONE',  ( -95.20000000000065654, -3.200000000000064126, -2.000000000000001776 ) ) ;
#9467 = LINE ( 'NONE', #14647, #9268 ) ;
#9468 = VERTEX_POINT ( 'NONE', #9750 ) ;
#9469 = FACE_OUTER_BOUND ( 'NONE', #16116, .T. ) ;
#9471 = VERTEX_POINT ( 'NONE', #6100 ) ;
#9470 = VERTEX_POINT ( 'NONE', #22446 ) ;
#9472 = ORIENTED_EDGE ( 'NONE', *, *, #9253, .F. ) ;
#9473 = ORIENTED_EDGE ( 'NONE', *, *, #1645, .F. ) ;
#9474 = CIRCLE ( 'NONE', #10955, 4.750000000000013323 ) ;
#9475 = ORIENTED_EDGE ( 'NONE', *, *, #16518, .T. ) ;
#9476 = VECTOR ( 'NONE', #15954, 1000.000000000000000 ) ;
#9477 = EDGE_CURVE ( 'NONE', #21352, #21116, #10612, .T. ) ;
#9478 = CYLINDRICAL_SURFACE ( 'NONE', #11809, 3.000000000000011546 ) ;
#9479 = B_SPLINE_CURVE_WITH_KNOTS ( 'NONE', 3,
 ( #1452, #2137, #2259, #14725, #20031, #19921 ),
 .UNSPECIFIED., .F., .F.,
 ( 4, 2, 4 ),
 ( 0.002044882221487538416, 0.003063384235218498917, 0.004081886248949459853 ),
 .UNSPECIFIED. ) ;
#9480 = CARTESIAN_POINT ( 'NONE',  ( 6.938893903907228378E-15, 4.618802153517023612, -3.433295621305385126 ) ) ;
#9481 = ORIENTED_EDGE ( 'NONE', *, *, #915, .F. ) ;
#9482 = CARTESIAN_POINT ( 'NONE',  ( 88.75737332930596324, -6.527605602963476805, 6.000000000000165201 ) ) ;
#9483 = VECTOR ( 'NONE', #3569, 1000.000000000000000 ) ;
#9484 = CARTESIAN_POINT ( 'NONE',  ( -4.211140560182305315, -2.431303136016589761, -3.745885042887437510 ) ) ;
#9485 = CARTESIAN_POINT ( 'NONE',  ( -1.354447211139180878E-14, -14.99999999999997513, 4.749999999999985789 ) ) ;
#9486 = CARTESIAN_POINT ( 'NONE',  ( -6.866595637048056311, 1.110223024625156540E-13, 27.70872448147268585 ) ) ;
#9487 = CARTESIAN_POINT ( 'NONE',  ( 8.697224362267997222, -1.499999999999984013, 6.250000000000005329 ) ) ;
#9488 = CARTESIAN_POINT ( 'NONE',  ( -7.029812747553743080, -13.37717092480936643, 8.933015330925142550 ) ) ;
#9489 = DIRECTION ( 'NONE',  ( 1.333893503340774882E-15, 2.778352770573747380E-17, 1.000000000000000000 ) ) ;
#9490 = AXIS2_PLACEMENT_3D ( 'NONE', #8764, #5246, #9004 ) ;
#9491 = CARTESIAN_POINT ( 'NONE',  ( 8.715898959466906959, -1.502431622389267751, 6.833978265954022469 ) ) ;
#9492 = CARTESIAN_POINT ( 'NONE',  ( -4.113620667976089607, 1.749999999999998002, -2.375000000000029754 ) ) ;
#9493 = AXIS2_PLACEMENT_3D ( 'NONE', #3593, #7016, #10527 ) ;
#9494 = TOROIDAL_SURFACE ( 'NONE', #11362, 1.750000000000000000, 0.2500000000000000000 ) ;
#9495 = PLANE ( 'NONE',  #14593 ) ;
#9496 = CARTESIAN_POINT ( 'NONE',  ( 4.052416734886668870, -1.393505408945144408, -3.567979131523768555 ) ) ;
#9497 = ORIENTED_EDGE ( 'NONE', *, *, #20189, .T. ) ;
#9498 = EDGE_CURVE ( 'NONE', #10170, #10973, #7984, .T. ) ;
#9499 = ORIENTED_EDGE ( 'NONE', *, *, #9835, .T. ) ;
#9500 = EDGE_CURVE ( 'NONE', #9648, #2950, #15497, .T. ) ;
#9501 = CARTESIAN_POINT ( 'NONE',  ( -52.60445557845683595, -2.775557561562891351E-14, 15.85914177512520773 ) ) ;
#9502 = DIRECTION ( 'NONE',  ( -9.693522803355793065E-26, 5.963788443470849249E-28, 1.000000000000000000 ) ) ;
#9503 = AXIS2_PLACEMENT_3D ( 'NONE', #21256, #3013, #1479 ) ;
#9504 = AXIS2_PLACEMENT_3D ( 'NONE', #19296, #18010, #15989 ) ;
#9505 = ORIENTED_EDGE ( 'NONE', *, *, #1757, .F. ) ;
#9506 = CIRCLE ( 'NONE', #21550, 0.5000000000000029976 ) ;
#9507 = DIRECTION ( 'NONE',  ( 1.000000000000000000, 1.871023177660678976E-14, 3.717264591378832268E-16 ) ) ;
#9508 = CIRCLE ( 'NONE', #17798, 2.999999999999995559 ) ;
#9509 = PLANE ( 'NONE',  #21280 ) ;
#9510 = CYLINDRICAL_SURFACE ( 'NONE', #21518, 0.5000000000000000000 ) ;
#9511 = AXIS2_PLACEMENT_3D ( 'NONE', #2974, #8273, #9920 ) ;
#9512 = DIRECTION ( 'NONE',  ( 0.000000000000000000, 0.000000000000000000, 1.000000000000000000 ) ) ;
#9513 = ADVANCED_FACE ( 'NONE', ( #13387 ), #11960, .F. ) ;
#9514 = LINE ( 'NONE', #11041, #21931 ) ;
#9515 = DIRECTION ( 'NONE',  ( -1.000000000000000000, -1.700709290173333260E-16, 0.000000000000000000 ) ) ;
#9516 = EDGE_CURVE ( 'NONE', #1131, #2262, #11735, .T. ) ;
#9517 = ORIENTED_EDGE ( 'NONE', *, *, #318, .F. ) ;
#9518 = DIRECTION ( 'NONE',  ( 1.424116703980846297E-16, -1.000000000000000000, 6.656013887802287108E-31 ) ) ;
#9519 = EDGE_CURVE ( 'NONE', #21618, #21696, #1604, .T. ) ;
#9520 = DIRECTION ( 'NONE',  ( -0.6819983600624998088, 0.7313537016191693496, 0.000000000000000000 ) ) ;
#9521 = DIRECTION ( 'NONE',  ( -1.066786462891689527E-26, -6.656013887802287108E-31, -1.000000000000000000 ) ) ;
#9522 = CARTESIAN_POINT ( 'NONE',  ( 0.2174200650117597278, -3.876582599186216171, -0.2855619784720702103 ) ) ;
#9523 = FACE_OUTER_BOUND ( 'NONE', #2273, .T. ) ;
#9524 = DIRECTION ( 'NONE',  ( 1.000000000000000000, -4.615739097524200579E-16, -1.134196829589820086E-15 ) ) ;
#9525 = DIRECTION ( 'NONE',  ( 1.858632295689435609E-16, 1.000000000000000000, -0.000000000000000000 ) ) ;
#9526 = AXIS2_PLACEMENT_3D ( 'NONE', #13521, #17029, #13754 ) ;
#9527 = CARTESIAN_POINT ( 'NONE',  ( 22.49999999999996092, 4.500000000000073719, -17.74999999999998224 ) ) ;
#9528 = CIRCLE ( 'NONE', #2384, 6.000000000000000000 ) ;
#9529 = TOROIDAL_SURFACE ( 'NONE', #17387, 1.300000000000000711, 0.5000000000000000000 ) ;
#9530 = TOROIDAL_SURFACE ( 'NONE', #5795, 1.000000000000000000, 0.5000000000000000000 ) ;
#9531 = EDGE_CURVE ( 'NONE', #1178, #11002, #20923, .T. ) ;
#9532 = AXIS2_PLACEMENT_3D ( 'NONE', #12131, #19321, #3215 ) ;
#9533 = ADVANCED_FACE ( 'NONE', ( #22564 ), #13624, .T. ) ;
#9534 = CONTEXT_DEPENDENT_SHAPE_REPRESENTATION ( #19600, #22637 ) ;
#9535 = ORIENTED_EDGE ( 'NONE', *, *, #4052, .F. ) ;
#9537 = ORIENTED_EDGE ( 'NONE', *, *, #943, .F. ) ;
#9536 = VERTEX_POINT ( 'NONE', #11853 ) ;
#9538 = ADVANCED_FACE ( 'NONE', ( #3035 ), #18802, .T. ) ;
#9539 = DIRECTION ( 'NONE',  ( -1.000000000000000000, 4.190823558986610327E-31, -1.733449886265890494E-32 ) ) ;
#9540 = CARTESIAN_POINT ( 'NONE',  ( 37.69139372032760349, 2.146704506890337223E-14, -2.221290437944543061 ) ) ;
#9541 = CARTESIAN_POINT ( 'NONE',  ( 8.697224362267972353, -12.00000000000004796, 6.250000000000059508 ) ) ;
#9542 = AXIS2_PLACEMENT_3D ( 'NONE', #3257, #10989, #4240 ) ;
#9544 = ORIENTED_EDGE ( 'NONE', *, *, #21914, .T. ) ;
#9543 = EDGE_CURVE ( 'NONE', #20452, #9827, #9859, .T. ) ;
#9545 = AXIS2_PLACEMENT_3D ( 'NONE', #5838, #6287, #18632 ) ;
#9546 = DIRECTION ( 'NONE',  ( -1.000000000000000000, 0.000000000000000000, 0.000000000000000000 ) ) ;
#9547 = DIRECTION ( 'NONE',  ( 0.7071067811865457964, 0.7071067811865492381, 0.000000000000000000 ) ) ;
#9548 = VECTOR ( 'NONE', #2042, 1000.000000000000000 ) ;
#9549 = ADVANCED_FACE ( 'NONE', ( #8451 ), #17250, .T. ) ;
#9550 = CARTESIAN_POINT ( 'NONE',  ( 4.151274195509686571, -2.039912954708743786, 3.533232880573495827 ) ) ;
#9551 = CARTESIAN_POINT ( 'NONE',  ( 0.02857727139927065951, -0.5999999999999898748, -3.398545894033815795 ) ) ;
#9552 = PLANE ( 'NONE',  #8705 ) ;
#9553 = CARTESIAN_POINT ( 'NONE',  ( 4.197393957002246268, 0.8151795401431507493, -3.503767560748920040 ) ) ;
#9554 = DIRECTION ( 'NONE',  ( 1.066786462891689527E-26, 6.656013887802287108E-31, 1.000000000000000000 ) ) ;
#9555 = LINE ( 'NONE', #6026, #17321 ) ;
#9556 = CARTESIAN_POINT ( 'NONE',  ( 6.999999999999992006, -5.999999999999981348, 10.74999999999998224 ) ) ;
#9557 = CYLINDRICAL_SURFACE ( 'NONE', #20605, 3.000000000000011546 ) ;
#9558 = B_SPLINE_CURVE_WITH_KNOTS ( 'NONE', 3,
 ( #2812, #2683, #6891, #23008, #3372, #6111, #10414, #9870, #21254, #15696, #21128, #20578, #22346, #12281 ),
 .UNSPECIFIED., .F., .F.,
 ( 4, 2, 2, 2, 2, 2, 4 ),
 ( 0.000000000000000000, 0.0008155857435326423210, 0.001223378615298963265, 0.001631171487065284642, 0.002038964358831601032, 0.002446757230597917422, 0.003262342974130546733 ),
 .UNSPECIFIED. ) ;
#9559 = CARTESIAN_POINT ( 'NONE',  ( -50.65685424949271720, -0.5000000000001045830, 7.500000000000076383 ) ) ;
#9560 = VERTEX_POINT ( 'NONE', #15490 ) ;
#9561 = AXIS2_PLACEMENT_3D ( 'NONE', #14374, #1559, #21571 ) ;
#9562 = AXIS2_PLACEMENT_3D ( 'NONE', #10148, #8384, #6616 ) ;
#9563 = CIRCLE ( 'NONE', #12563, 7.000000000000075495 ) ;
#9565 = VERTEX_POINT ( 'NONE', #22688 ) ;
#9564 = ORIENTED_EDGE ( 'NONE', *, *, #20056, .T. ) ;
#9566 = VECTOR ( 'NONE', #182, 999.9999999999998863 ) ;
#9567 = ORIENTED_EDGE ( 'NONE', *, *, #1648, .F. ) ;
#9568 = ORIENTED_EDGE ( 'NONE', *, *, #8436, .F. ) ;
#9570 = VERTEX_POINT ( 'NONE', #10780 ) ;
#9569 = ORIENTED_EDGE ( 'NONE', *, *, #18133, .F. ) ;
#9571 = VERTEX_POINT ( 'NONE', #22919 ) ;
#9572 = EDGE_CURVE ( 'NONE', #635, #10026, #9392, .T. ) ;
#9573 = DIRECTION ( 'NONE',  ( 1.665334536937736980E-15, 0.000000000000000000, 1.000000000000000000 ) ) ;
#9574 = EDGE_LOOP ( 'NONE', ( #15874, #12979, #7911, #20067 ) ) ;
#9575 = VERTEX_POINT ( 'NONE', #4898 ) ;
#9576 = FILL_AREA_STYLE_COLOUR ( '', #18584 ) ;
#9577 = CARTESIAN_POINT ( 'NONE',  ( 0.2174200650117701361, -3.876582599186239264, -0.2855619784720585530 ) ) ;
#9578 = CARTESIAN_POINT ( 'NONE',  ( 0.000000000000000000, 0.000000000000000000, -3.499999999999996003 ) ) ;
#9579 = DIRECTION ( 'NONE',  ( 1.733449886265891589E-32, -4.190823558986610327E-31, 1.000000000000000000 ) ) ;
#9580 = EDGE_CURVE ( 'NONE', #10962, #3180, #12064, .T. ) ;
#9581 = AXIS2_PLACEMENT_3D ( 'NONE', #13076, #20135, #2252 ) ;
#9582 = CARTESIAN_POINT ( 'NONE',  ( -4.211140560182305315, -2.431303136016589761, -3.745885042887437510 ) ) ;
#9583 = AXIS2_PLACEMENT_3D ( 'NONE', #17428, #23099, #14021 ) ;
#9584 = CARTESIAN_POINT ( 'NONE',  ( 0.4637351969133408636, 1.749999999999980904, -4.750000000000024869 ) ) ;
#9585 = DIRECTION ( 'NONE',  ( 0.000000000000000000, 0.000000000000000000, 1.000000000000000000 ) ) ;
#9586 = SURFACE_STYLE_FILL_AREA ( #20293 ) ;
#9587 = DIRECTION ( 'NONE',  ( -7.395570986446975166E-31, -3.382522293539642681E-32, -1.000000000000000000 ) ) ;
#9588 = CARTESIAN_POINT ( 'NONE',  ( 37.22062532321636752, 10.88440674090231219, -2.456674636499794673 ) ) ;
#9589 = ORIENTED_EDGE ( 'NONE', *, *, #883, .T. ) ;
#9590 = PRESENTATION_STYLE_ASSIGNMENT (( #12882 ) ) ;
#9591 = CARTESIAN_POINT ( 'NONE',  ( 6.500000000000172307, -13.52760560296348302, -2.081668171172168513E-14 ) ) ;
#9593 = VERTEX_POINT ( 'NONE', #17609 ) ;
#9592 = ORIENTED_EDGE ( 'NONE', *, *, #14711, .F. ) ;
#9594 = EDGE_LOOP ( 'NONE', ( #21082, #11337, #15966, #6755, #19932 ) ) ;
#9595 = AXIS2_PLACEMENT_3D ( 'NONE', #18931, #2813, #18684 ) ;
#9596 = ORIENTED_EDGE ( 'NONE', *, *, #21040, .T. ) ;
#9597 = AXIS2_PLACEMENT_3D ( 'NONE', #2830, #15283, #15047 ) ;
#9598 = EDGE_CURVE ( 'NONE', #1919, #4144, #2716, .T. ) ;
#9599 = ORIENTED_EDGE ( 'NONE', *, *, #1358, .F. ) ;
#9600 = FACE_OUTER_BOUND ( 'NONE', #10688, .T. ) ;
#9601 = LINE ( 'NONE', #1014, #1620 ) ;
#9602 = VERTEX_POINT ( 'NONE', #17851 ) ;
#9603 = EDGE_CURVE ( 'NONE', #20996, #5042, #13852, .T. ) ;
#9604 = LINE ( 'NONE', #4070, #459 ) ;
#9605 = CARTESIAN_POINT ( 'NONE',  ( -12.85000000000005649, -12.50000000000011191, -6.249999999999921840 ) ) ;
#9606 = AXIS2_PLACEMENT_3D ( 'NONE', #5274, #10447, #17053 ) ;
#9607 = CARTESIAN_POINT ( 'NONE',  ( -12.84999999999999964, -2.000000000000001776, 0.000000000000000000 ) ) ;
#9608 = CARTESIAN_POINT ( 'NONE',  ( 81.04599508018871745, -4.805938895142302769, 6.500000000000144773 ) ) ;
#9609 = CARTESIAN_POINT ( 'NONE',  ( -8.129778652391308924, -12.42126101213639444, 7.405931224841348026 ) ) ;
#9610 = DIRECTION ( 'NONE',  ( -1.000000000000000000, 0.000000000000000000, -3.717264591378832268E-16 ) ) ;
#9611 = CYLINDRICAL_SURFACE ( 'NONE', #344, 2.549999999999998934 ) ;
#9612 = LINE ( 'NONE', #11256, #12523 ) ;
#9613 = CARTESIAN_POINT ( 'NONE',  ( 37.43301270189240171, 0.2499999999999834577, -10.00000000000006573 ) ) ;
#9614 = EDGE_CURVE ( 'NONE', #17626, #6390, #18882, .T. ) ;
#9615 =( NAMED_UNIT ( * ) PLANE_ANGLE_UNIT ( ) SI_UNIT ( $, .RADIAN. ) );
#9616 = DIRECTION ( 'NONE',  ( 0.7071067811865460184, -0.7071067811865490160, -1.010793663541200360E-16 ) ) ;
#9617 = DIRECTION ( 'NONE',  ( -1.000000000000000000, -6.224605580259554159E-31, 2.887593071917436153E-31 ) ) ;
#9618 = ORIENTED_EDGE ( 'NONE', *, *, #8072, .T. ) ;
#9619 = COLOUR_RGB ( '', 0.40784314, 0.44705882, 0.49803922) ;
#9620 = ORIENTED_EDGE ( 'NONE', *, *, #10397, .F. ) ;
#9621 = ORIENTED_EDGE ( 'NONE', *, *, #18243, .T. ) ;
#9622 = ORIENTED_EDGE ( 'NONE', *, *, #21029, .F. ) ;
#9623 = DIRECTION ( 'NONE',  ( -5.551115123561405253E-17, -1.000000000000000000, -2.256980353643891447E-27 ) ) ;
#9624 = CARTESIAN_POINT ( 'NONE',  ( -4.000000000000003553, -0.3902508023145539462, -5.599999999999998757 ) ) ;
#9625 = EDGE_LOOP ( 'NONE', ( #12642, #17294, #16894, #1545, #21924, #21079 ) ) ;
#9626 = AXIS2_PLACEMENT_3D ( 'NONE', #10531, #10071, #17233 ) ;
#9627 = DIRECTION ( 'NONE',  ( 5.551115123125761132E-17, -1.577721810442025713E-30, 1.000000000000000000 ) ) ;
#9628 = CARTESIAN_POINT ( 'NONE',  ( 37.86602540378461157, 11.00000000000000000, -2.133974596215532316 ) ) ;
#9629 = DIRECTION ( 'NONE',  ( 0.1556420233463033653, 0.000000000000000000, 0.9878135252003128475 ) ) ;
#9630 = DIRECTION ( 'NONE',  ( 3.330669073875432643E-16, 4.437342591868153746E-31, -1.000000000000000000 ) ) ;
#9631 = CARTESIAN_POINT ( 'NONE',  ( 4.690415759823449271, 0.7500000000000559552, -2.132316638858528624 ) ) ;
#9632 = CARTESIAN_POINT ( 'NONE',  ( 7.126417736726686769, -13.56697759857014418, 8.494066294656340332 ) ) ;
#9633 = DIRECTION ( 'NONE',  ( -0.9878135252003118483, -1.429810390713075314E-30, 0.1556420233463089442 ) ) ;
#9634 = CARTESIAN_POINT ( 'NONE',  ( -6.000000000000116351, 5.299999999999957190, -7.500000000000062172 ) ) ;
#9635 = FACE_OUTER_BOUND ( 'NONE', #6754, .T. ) ;
#9636 = CYLINDRICAL_SURFACE ( 'NONE', #10464, 2.550000000000012701 ) ;
#9637 =( LENGTH_UNIT ( ) NAMED_UNIT ( * ) SI_UNIT ( .MILLI., .METRE. ) );
#9638 = EDGE_CURVE ( 'NONE', #9218, #19862, #10438, .T. ) ;
#9639 = FACE_OUTER_BOUND ( 'NONE', #20302, .T. ) ;
#9640 = B_SPLINE_CURVE_WITH_KNOTS ( 'NONE', 3,
 ( #11420, #8131, #2838, #2479, #18958, #10014 ),
 .UNSPECIFIED., .F., .F.,
 ( 4, 2, 4 ),
 ( 0.002044882221487566605, 0.003063384235218515397, 0.004081886248949463322 ),
 .UNSPECIFIED. ) ;
#9641 = VERTEX_POINT ( 'NONE', #17488 ) ;
#9642 = EDGE_CURVE ( 'NONE', #172, #7692, #2385, .T. ) ;
#9643 = ITEM_DEFINED_TRANSFORMATION ( 'NONE', 'NONE', #7882,  #22115 ) ;
#9644 = EDGE_LOOP ( 'NONE', ( #2610, #17656, #21610, #7739 ) ) ;
#9645 = EDGE_CURVE ( 'NONE', #14161, #3914, #3801, .T. ) ;
#9646 = CIRCLE ( 'NONE', #13041, 0.4999999999999982236 ) ;
#9648 = VERTEX_POINT ( 'NONE', #12188 ) ;
#9647 = EDGE_LOOP ( 'NONE', ( #20545, #6952, #17760 ) ) ;
#9649 = FACE_OUTER_BOUND ( 'NONE', #2055, .T. ) ;
#9650 = CARTESIAN_POINT ( 'NONE',  ( 1.849731447979666488, -1.560358803171614461, -4.750000000000024869 ) ) ;
#9651 = FILL_AREA_STYLE ('',( #16804 ) ) ;
#9652 = ORIENTED_EDGE ( 'NONE', *, *, #567, .T. ) ;
#9653 = DIRECTION ( 'NONE',  ( 3.241725282392603095E-30, 1.000000000000000000, -2.218671295934100958E-31 ) ) ;
#9654 = DIRECTION ( 'NONE',  ( 3.862887998903635106E-15, -0.5454545454545466354, 0.8381404052084434619 ) ) ;
#9655 = CARTESIAN_POINT ( 'NONE',  ( 4.170895651974850793, -2.054890354522706186, 3.559174498016318466 ) ) ;
#9657 = EDGE_CURVE ( 'NONE', #226, #18733, #14186, .T. ) ;
#9656 = CARTESIAN_POINT ( 'NONE',  ( -5.122455540400322249, 36.64919863988808402, -16.21011172720200477 ) ) ;
#9658 = CARTESIAN_POINT ( 'NONE',  ( 1.387778780781445676E-14, 4.618802153517020059, -5.242734410091827613 ) ) ;
#9659 = DIRECTION ( 'NONE',  ( -1.000000000000000000, 0.000000000000000000, 0.000000000000000000 ) ) ;
#9660 = CARTESIAN_POINT ( 'NONE',  ( 0.000000000000000000, 0.000000000000000000, -5.600000000000000533 ) ) ;
#9661 = CARTESIAN_POINT ( 'NONE',  ( 0.000000000000000000, 1.387778780781445676E-14, 17.24999999999997513 ) ) ;
#9662 = AXIS2_PLACEMENT_3D ( 'NONE', #1381, #6326, #4778 ) ;
#9663 = ADVANCED_FACE ( 'NONE', ( #3496 ), #17723, .T. ) ;
#9664 = CIRCLE ( 'NONE', #6283, 0.4999999999999995559 ) ;
#9665 = FACE_OUTER_BOUND ( 'NONE', #19593, .T. ) ;
#9666 = FILL_AREA_STYLE ('',( #11304 ) ) ;
#9667 = DIRECTION ( 'NONE',  ( -1.000000000000000000, 9.957992501029406452E-17, 2.655250634480538332E-32 ) ) ;
#9668 = DIRECTION ( 'NONE',  ( 9.121204216617949000E-31, 1.000000000000000000, -6.982962677686261977E-15 ) ) ;
#9669 = VERTEX_POINT ( 'NONE', #19609 ) ;
#9670 = AXIS2_PLACEMENT_3D ( 'NONE', #21166, #1514, #14220 ) ;
#9671 = EDGE_CURVE ( 'NONE', #21212, #6874, #6109, .T. ) ;
#9672 = EDGE_CURVE ( 'NONE', #19569, #16720, #3273, .T. ) ;
#9674 = ORIENTED_EDGE ( 'NONE', *, *, #13156, .F. ) ;
#9673 = ORIENTED_EDGE ( 'NONE', *, *, #3757, .T. ) ;
#9675 = VECTOR ( 'NONE', #18290, 1000.000000000000000 ) ;
#9676 = ORIENTED_EDGE ( 'NONE', *, *, #3742, .F. ) ;
#9677 = VERTEX_POINT ( 'NONE', #5143 ) ;
#9679 = ORIENTED_EDGE ( 'NONE', *, *, #8260, .F. ) ;
#9678 = EDGE_LOOP ( 'NONE', ( #9852, #4307, #20517, #16604 ) ) ;
#9680 = CIRCLE ( 'NONE', #18315, 2.000000000000001776 ) ;
#9681 = ORIENTED_EDGE ( 'NONE', *, *, #23225, .F. ) ;
#9682 = CARTESIAN_POINT ( 'NONE',  ( -4.692963726980094563, -1.672424706883767875, 1.371548386792662333 ) ) ;
#9683 = VECTOR ( 'NONE', #11200, 1000.000000000000000 ) ;
#9684 = CARTESIAN_POINT ( 'NONE',  ( 0.000000000000000000, 0.000000000000000000, 0.000000000000000000 ) ) ;
#9685 = ORIENTED_EDGE ( 'NONE', *, *, #20454, .T. ) ;
#9686 = CARTESIAN_POINT ( 'NONE',  ( 4.071447262713884463, 2.020725942163681399, 3.499999999999996003 ) ) ;
#9687 = CARTESIAN_POINT ( 'NONE',  ( -50.65685424949267457, -2.700000000000091216, -7.500000000000034639 ) ) ;
#9688 = CARTESIAN_POINT ( 'NONE',  ( -2.700000000000063238, 4.799999999999935874, 8.000000000000062172 ) ) ;
#9689 = AXIS2_PLACEMENT_3D ( 'NONE', #15495, #8220, #11859 ) ;
#9690 = LINE ( 'NONE', #10151, #8637 ) ;
#9691 = ADVANCED_FACE ( 'NONE', ( #15950 ), #16224, .T. ) ;
#9692 = CARTESIAN_POINT ( 'NONE',  ( -7.499999999999989342, -2.428697021683995594, 9.041853041250330847 ) ) ;
#9693 = VECTOR ( 'NONE', #8772, 1000.000000000000000 ) ;
#9694 = AXIS2_PLACEMENT_3D ( 'NONE', #10271, #22869, #4973 ) ;
#9695 = EDGE_CURVE ( 'NONE', #15040, #3943, #5377, .T. ) ;
#9696 = DIRECTION ( 'NONE',  ( -1.000000000000000000, 7.100545512326564696E-57, 1.066786462891689527E-26 ) ) ;
#9697 = DIRECTION ( 'NONE',  ( -0.9706398123736330597, -2.155253336630096709E-16, -0.2405376366294442736 ) ) ;
#9698 = AXIS2_PLACEMENT_3D ( 'NONE', #1020, #22422, #20670 ) ;
#9699 = DIRECTION ( 'NONE',  ( -1.066786462891689527E-26, -6.656013887802287108E-31, -1.000000000000000000 ) ) ;
#9700 = CARTESIAN_POINT ( 'NONE',  ( 24.75000000000000355, 2.000000000000029310, -1.250000000000004663 ) ) ;
#9701 = DIRECTION ( 'NONE',  ( -2.172745813409348851E-17, 1.000000000000000000, 3.406761633869148826E-16 ) ) ;
#9702 = DIRECTION ( 'NONE',  ( 1.066788928082016908E-26, 3.471809175856251779E-58, -1.000000000000000000 ) ) ;
#9703 = CARTESIAN_POINT ( 'NONE',  ( 5.599999999999994316, 4.041451884327383226, -1.734723475976807094E-15 ) ) ;
#9704 = ADVANCED_FACE ( 'NONE', ( #20309 ), #11244, .F. ) ;
#9705 = DIRECTION ( 'NONE',  ( 6.656013887802287108E-31, 1.000000000000000000, -3.469446951953609061E-15 ) ) ;
#9706 = AXIS2_PLACEMENT_3D ( 'NONE', #18723, #11654, #2714 ) ;
#9707 = VERTEX_POINT ( 'NONE', #9480 ) ;
#9708 = ADVANCED_FACE ( 'NONE', ( #21842 ), #4172, .F. ) ;
#9709 = FILL_AREA_STYLE ('',( #8054 ) ) ;
#9711 = VERTEX_POINT ( 'NONE', #14889 ) ;
#9710 = VERTEX_POINT ( 'NONE', #16520 ) ;
#9712 = ORIENTED_EDGE ( 'NONE', *, *, #10549, .F. ) ;
#9713 = AXIS2_PLACEMENT_3D ( 'NONE', #10926, #14127, #134 ) ;
#9714 = VERTEX_POINT ( 'NONE', #11006 ) ;
#9715 = AXIS2_PLACEMENT_3D ( 'NONE', #18116, #1539, #12705 ) ;
#9716 = CIRCLE ( 'NONE', #716, 5.371010071662839280 ) ;
#9717 = VERTEX_POINT ( 'NONE', #5962 ) ;
#9718 = VERTEX_POINT ( 'NONE', #16638 ) ;
#9719 = CARTESIAN_POINT ( 'NONE',  ( 0.000000000000000000, 0.000000000000000000, -0.2800830152838822418 ) ) ;
#9720 = DIRECTION ( 'NONE',  ( -0.7071067811865462405, -3.140184917367542938E-16, 0.7071067811865489050 ) ) ;
#9721 = VERTEX_POINT ( 'NONE', #431 ) ;
#9722 =( GEOMETRIC_REPRESENTATION_CONTEXT ( 3 ) GLOBAL_UNCERTAINTY_ASSIGNED_CONTEXT ( ( #22732 ) ) GLOBAL_UNIT_ASSIGNED_CONTEXT ( ( #4279, #19951, #656 ) ) REPRESENTATION_CONTEXT ( 'NONE', 'WORKASPACE' ) );
#9723 = CARTESIAN_POINT ( 'NONE',  ( 4.170895651974849905, -4.109780709045238289, -6.938019423604825320E-15 ) ) ;
#9724 = CYLINDRICAL_SURFACE ( 'NONE', #6863, 2.550000000000003819 ) ;
#9725 = FACE_OUTER_BOUND ( 'NONE', #17422, .T. ) ;
#9726 = CARTESIAN_POINT ( 'NONE',  ( 0.000000000000000000, -14.99999999999997513, -1.387778780781445676E-14 ) ) ;
#9727 = FACE_OUTER_BOUND ( 'NONE', #2036, .T. ) ;
#9728 = ADVANCED_FACE ( 'NONE', ( #18536 ), #9025, .F. ) ;
#9729 = CARTESIAN_POINT ( 'NONE',  ( -7.282868595548766422, -13.73825694947798581, 8.010178330700920668 ) ) ;
#9730 = AXIS2_PLACEMENT_3D ( 'NONE', #19860, #7170, #16318 ) ;
#9731 = FACE_OUTER_BOUND ( 'NONE', #18841, .T. ) ;
#9732 = CARTESIAN_POINT ( 'NONE',  ( -3.999999999708153453, 42.99999999900385461, -15.50000000000000000 ) ) ;
#9733 = LINE ( 'NONE', #8076, #21298 ) ;
#9734 = PRESENTATION_STYLE_ASSIGNMENT (( #7962 ) ) ;
#9735 = CARTESIAN_POINT ( 'NONE',  ( 12.49999999999995914, 0.2500000000000002220, -4.750000000000002665 ) ) ;
#9736 = DIRECTION ( 'NONE',  ( 0.000000000000000000, -4.190823558986610327E-31, 1.000000000000000000 ) ) ;
#9737 = VERTEX_POINT ( 'NONE', #18310 ) ;
#9738 = B_SPLINE_CURVE_WITH_KNOTS ( 'NONE', 3,
 ( #3097, #21453, #12481, #5322, #5210, #1337, #19325, #10725, #12369, #15660, #19552, #1219, #22860, #6737 ),
 .UNSPECIFIED., .F., .F.,
 ( 4, 2, 2, 2, 2, 2, 4 ),
 ( 2.826448204503814216E-21, 0.001011182963765816078, 0.001516774445648722165, 0.002022365927531628253, 0.002527957409414534340, 0.003033548891297440427, 0.004044731855063248699 ),
 .UNSPECIFIED. ) ;
#9739 = EDGE_CURVE ( 'NONE', #12565, #22996, #316, .T. ) ;
#9740 = MECHANICAL_DESIGN_GEOMETRIC_PRESENTATION_REPRESENTATION (  '', ( #15720 ), #11588 ) ;
#9741 = ORIENTED_EDGE ( 'NONE', *, *, #20596, .T. ) ;
#9742 = EDGE_LOOP ( 'NONE', ( #12865, #12823, #15685, #2616 ) ) ;
#9743 = VERTEX_POINT ( 'NONE', #13135 ) ;
#9744 = ORIENTED_EDGE ( 'NONE', *, *, #12634, .F. ) ;
#9745 = CARTESIAN_POINT ( 'NONE',  ( 3.951447005078448260, 3.704664227300101587, 0.5833333333333330373 ) ) ;
#9746 = CIRCLE ( 'NONE', #8233, 0.5000000000000038858 ) ;
#9747 = DIRECTION ( 'NONE',  ( 1.000000000000000000, 0.000000000000000000, 0.000000000000000000 ) ) ;
#9748 = ORIENTED_EDGE ( 'NONE', *, *, #6520, .F. ) ;
#9749 = AXIS2_PLACEMENT_3D ( 'NONE', #7273, #16309, #6798 ) ;
#9750 = CARTESIAN_POINT ( 'NONE',  ( 2.499999999999988454, 4.500000000000059508, -0.2500000000000349165 ) ) ;
#9751 = DIRECTION ( 'NONE',  ( -1.000000000000000000, -4.440892098500626162E-16, 5.551115123125782702E-16 ) ) ;
#9752 = DIRECTION ( 'NONE',  ( 0.000000000000000000, 0.000000000000000000, 1.000000000000000000 ) ) ;
#9753 = CARTESIAN_POINT ( 'NONE',  ( -6.605954977391715666, 35.99999999900384751, -18.74919553276986761 ) ) ;
#9754 = CARTESIAN_POINT ( 'NONE',  ( -4.154094228333751637, -2.398367420967737917, -3.721909803043223164 ) ) ;
#9755 = DIRECTION ( 'NONE',  ( -1.550910762415566494E-16, -1.000000000000000000, 8.135128085091684243E-31 ) ) ;
#9756 = DIRECTION ( 'NONE',  ( 0.000000000000000000, 6.938893903907245733E-15, 1.000000000000000000 ) ) ;
#9757 = FACE_OUTER_BOUND ( 'NONE', #18098, .T. ) ;
#9758 = DIRECTION ( 'NONE',  ( -1.000000000000000000, 2.833381677428764831E-14, 0.000000000000000000 ) ) ;
#9759 = CARTESIAN_POINT ( 'NONE',  ( 119.5756419024615269, -4.000000000000003553, 6.500000000000123457 ) ) ;
#9760 = CARTESIAN_POINT ( 'NONE',  ( 37.43301270189236618, 10.75000000000000000, -2.999999999999988898 ) ) ;
#9761 = CARTESIAN_POINT ( 'NONE',  ( 37.18301270189234486, 0.09150635094609947673, -2.475480947161597278 ) ) ;
#9762 = CARTESIAN_POINT ( 'NONE',  ( 4.158413352280815545, 2.044871626972824430, -3.541821552872970180 ) ) ;
#9763 = CONTEXT_DEPENDENT_SHAPE_REPRESENTATION ( #16149, #21147 ) ;
#9764 = ORIENTED_EDGE ( 'NONE', *, *, #6786, .F. ) ;
#9765 = AXIS2_PLACEMENT_3D ( 'NONE', #22728, #13671, #4246 ) ;
#9767 = EDGE_LOOP ( 'NONE', ( #5198, #20893, #8290, #15453 ) ) ;
#9766 = EDGE_LOOP ( 'NONE', ( #10286, #9475, #20916, #3294 ) ) ;
#9768 = FACE_OUTER_BOUND ( 'NONE', #10189, .T. ) ;
#9769 = CARTESIAN_POINT ( 'NONE',  ( 5.599999999999994316, 2.020725942163688504, 3.499999999999997780 ) ) ;
#9770 = ADVANCED_FACE ( 'NONE', ( #11124 ), #5497, .F. ) ;
#9771 = VERTEX_POINT ( 'NONE', #12656 ) ;
#9772 = CARTESIAN_POINT ( 'NONE',  ( -49.51923881554284890, -1.137615433949877630, 8.000000000000076383 ) ) ;
#9773 = DIRECTION ( 'NONE',  ( 1.927470528863118556E-16, 1.000000000000000000, -7.131640956793539050E-15 ) ) ;
#9774 = CARTESIAN_POINT ( 'NONE',  ( -3.999999999708153453, 35.49999999900384751, -22.50000000000000000 ) ) ;
#9775 = CYLINDRICAL_SURFACE ( 'NONE', #12603, 0.5000000000000004441 ) ;
#9776 = FACE_OUTER_BOUND ( 'NONE', #6157, .T. ) ;
#9777 = AXIS2_PLACEMENT_3D ( 'NONE', #8502, #17665, #1556 ) ;
#9778 = CARTESIAN_POINT ( 'NONE',  ( 31.55000000029185259, 16.99999999900385461, -26.00000000000000000 ) ) ;
#9779 = SURFACE_STYLE_USAGE ( .BOTH. , #9437 ) ;
#9780 = CARTESIAN_POINT ( 'NONE',  ( 10.50000000000000888, -1.500000000000001332, 9.250000000000008882 ) ) ;
#9781 = CARTESIAN_POINT ( 'NONE',  ( 0.1217565302851174314, 3.710888496608926612, -0.5725525826505064586 ) ) ;
#9782 = CYLINDRICAL_SURFACE ( 'NONE', #699, 2.499999999999993339 ) ;
#9783 = CARTESIAN_POINT ( 'NONE',  ( -4.000000000000098588, 1.539600717839030741, -3.300726591567078483 ) ) ;
#9784 = DIRECTION ( 'NONE',  ( -1.000000000000000000, 1.025846074753645022E-13, 0.000000000000000000 ) ) ;
#9785 = VERTEX_POINT ( 'NONE', #19843 ) ;
#9786 = PRESENTATION_STYLE_ASSIGNMENT (( #1202 ) ) ;
#9788 = VERTEX_POINT ( 'NONE', #5731 ) ;
#9787 = ORIENTED_EDGE ( 'NONE', *, *, #17419, .T. ) ;
#9789 = UNCERTAINTY_MEASURE_WITH_UNIT (LENGTH_MEASURE( 1.000000000000000082E-05 ), #15597, 'distance_accuracy_value', 'NONE');
#9790 = EDGE_LOOP ( 'NONE', ( #2940, #10253, #1914, #3882 ) ) ;
#9791 = ADVANCED_FACE ( 'NONE', ( #554 ), #18204, .T. ) ;
#9793 = EDGE_LOOP ( 'NONE', ( #18593, #307, #309, #12594 ) ) ;
#9792 = ORIENTED_EDGE ( 'NONE', *, *, #21051, .T. ) ;
#9794 = AXIS2_PLACEMENT_3D ( 'NONE', #18952, #22482, #17166 ) ;
#9795 = ORIENTED_EDGE ( 'NONE', *, *, #19503, .T. ) ;
#9796 = CARTESIAN_POINT ( 'NONE',  ( 85.68838070902461368, -9.818697260249752645, -6.000000000000032863 ) ) ;
#9797 = DIRECTION ( 'NONE',  ( -1.000000000000000000, -2.699383410053119644E-30, -3.330669073875432643E-16 ) ) ;
#9798 = ADVANCED_FACE ( 'NONE', ( #3829 ), #12870, .T. ) ;
#9799 = ORIENTED_EDGE ( 'NONE', *, *, #21470, .F. ) ;
#9800 =( NAMED_UNIT ( * ) SI_UNIT ( $, .STERADIAN. ) SOLID_ANGLE_UNIT ( ) );
#9801 = DIRECTION ( 'NONE',  ( -9.121204216617949000E-31, -1.000000000000000000, 6.982962677686261977E-15 ) ) ;
#9802 = B_SPLINE_CURVE_WITH_KNOTS ( 'NONE', 3,
 ( #2955, #13661, #4478, #17524, #11647, #15296 ),
 .UNSPECIFIED., .F., .F.,
 ( 4, 2, 4 ),
 ( 0.002336974151641598059, 0.003500975885716476645, 0.004664977619791355230 ),
 .UNSPECIFIED. ) ;
#9803 = DIRECTION ( 'NONE',  ( -0.000000000000000000, -0.000000000000000000, 1.000000000000000000 ) ) ;
#9804 = DIRECTION ( 'NONE',  ( 2.013525853228507892E-32, 6.902532920683810383E-31, -1.000000000000000000 ) ) ;
#9805 = DIRECTION ( 'NONE',  ( 0.000000000000000000, 1.000000000000000000, 0.000000000000000000 ) ) ;
#9806 = EDGE_CURVE ( 'NONE', #17095, #12860, #7489, .T. ) ;
#9807 = CARTESIAN_POINT ( 'NONE',  ( 3.999999999998528288, 1.658577278524556942, -3.531553309553837838 ) ) ;
#9808 = CARTESIAN_POINT ( 'NONE',  ( 7.778057173929710189, -1.762098510204312518, 7.981635986975429198 ) ) ;
#9809 = EDGE_CURVE ( 'NONE', #8293, #6413, #13632, .T. ) ;
#9810 = CARTESIAN_POINT ( 'NONE',  ( 3.878089031707351086, 0.7015470581927514271, 3.499999999999968914 ) ) ;
#9811 = CARTESIAN_POINT ( 'NONE',  ( 24.74999999999994316, 6.938893903907228378E-14, -17.00000000000001066 ) ) ;
#9812 = LINE ( 'NONE', #4385, #19825 ) ;
#9813 = LINE ( 'NONE', #18867, #9343 ) ;
#9814 = VECTOR ( 'NONE', #21969, 1000.000000000000000 ) ;
#9815 = DIRECTION ( 'NONE',  ( -4.615739097524193676E-16, 1.000000000000000000, -4.560992131517923160E-31 ) ) ;
#9816 = CARTESIAN_POINT ( 'NONE',  ( -65.47859922179033276, 2.700000000000056577, -11.38422848940298593 ) ) ;
#9817 = ORIENTED_EDGE ( 'NONE', *, *, #4461, .F. ) ;
#9818 =( NAMED_UNIT ( * ) SI_UNIT ( $, .STERADIAN. ) SOLID_ANGLE_UNIT ( ) );
#9820 = ORIENTED_EDGE ( 'NONE', *, *, #6538, .F. ) ;
#9819 = ORIENTED_EDGE ( 'NONE', *, *, #20733, .F. ) ;
#9821 = EDGE_CURVE ( 'NONE', #13336, #19106, #16610, .T. ) ;
#9822 = ORIENTED_EDGE ( 'NONE', *, *, #22898, .T. ) ;
#9823 = EDGE_CURVE ( 'NONE', #3943, #16034, #5853, .T. ) ;
#9824 = EDGE_CURVE ( 'NONE', #4649, #18414, #22654, .T. ) ;
#9825 = ORIENTED_EDGE ( 'NONE', *, *, #5661, .T. ) ;
#9826 = EDGE_LOOP ( 'NONE', ( #5168, #10056, #12330 ) ) ;
#9827 = VERTEX_POINT ( 'NONE', #2532 ) ;
#9828 = CARTESIAN_POINT ( 'NONE',  ( 4.093692494532773729, -2.021783646005764101, 3.501831996793847157 ) ) ;
#9829 = CONICAL_SURFACE ( 'NONE', #10207, 7.500000000000001776, 1.308996938995750092 ) ;
#9830 = CARTESIAN_POINT ( 'NONE',  ( 80.49335071782266482, -7.708908342713538531, 6.000000000000081712 ) ) ;
#9831 = EDGE_CURVE ( 'NONE', #9302, #2116, #10222, .T. ) ;
#9832 = ORIENTED_EDGE ( 'NONE', *, *, #7095, .T. ) ;
#9833 = DIRECTION ( 'NONE',  ( 0.000000000000000000, 1.000000000000000000, 0.000000000000000000 ) ) ;
#9834 = SHAPE_REPRESENTATION ( 'hex nut gradec_bsi_BS EN 24034 - M5 - N', ( #22115 ), #2988 ) ;
#9835 = EDGE_CURVE ( 'NONE', #16088, #16004, #3102, .T. ) ;
#9836 = DIRECTION ( 'NONE',  ( 1.424116703980846297E-16, -1.000000000000000000, 6.656013887802287108E-31 ) ) ;
#9837 = DIRECTION ( 'NONE',  ( -2.013525853228507892E-32, -6.902532920683810383E-31, 1.000000000000000000 ) ) ;
#9838 = DIRECTION ( 'NONE',  ( -1.000000000000000000, 2.168404344971005170E-16, -1.203141491611682442E-30 ) ) ;
#9839 = CARTESIAN_POINT ( 'NONE',  ( -8.954763739086832430, -12.00000000000004263, 6.678571428571464352 ) ) ;
#9840 = CARTESIAN_POINT ( 'NONE',  ( 1.387778780781445676E-14, 4.163336342344337027E-14, -2.000000000000001776 ) ) ;
#9841 = FACE_BOUND ( 'NONE', #5103, .T. ) ;
#9842 = DIRECTION ( 'NONE',  ( -3.254448077146059901E-32, -1.000000000000000000, -6.409494854920712161E-31 ) ) ;
#9843 = ORIENTED_EDGE ( 'NONE', *, *, #14869, .F. ) ;
#9844 =( NAMED_UNIT ( * ) PLANE_ANGLE_UNIT ( ) SI_UNIT ( $, .RADIAN. ) );
#9845 = CARTESIAN_POINT ( 'NONE',  ( 4.055492966679643096, 2.385006769473020150, 3.005124364834455442 ) ) ;
#9847 = AXIS2_PLACEMENT_3D ( 'NONE', #5903, #21904, #11192 ) ;
#9846 = DIRECTION ( 'NONE',  ( -1.000000000000000000, 4.615739097524200579E-16, 1.134196829589820086E-15 ) ) ;
#9848 = AXIS2_PLACEMENT_3D ( 'NONE', #14803, #5874, #18678 ) ;
#9849 = EDGE_LOOP ( 'NONE', ( #5823, #15310, #19839, #22682 ) ) ;
#9850 = EDGE_LOOP ( 'NONE', ( #2792, #10337, #13597, #13477 ) ) ;
#9851 = ORIENTED_EDGE ( 'NONE', *, *, #21677, .F. ) ;
#9852 = ORIENTED_EDGE ( 'NONE', *, *, #9391, .T. ) ;
#9853 = PRODUCT_DEFINITION_SHAPE ( 'NONE', 'NONE',  #23288 ) ;
#9854 = ORIENTED_EDGE ( 'NONE', *, *, #6241, .F. ) ;
#9855 = CARTESIAN_POINT ( 'NONE',  ( -50.65685424949274562, -1.040834085586084257E-13, 8.000000000000062172 ) ) ;
#9856 = DIRECTION ( 'NONE',  ( 0.000000000000000000, 0.000000000000000000, 1.000000000000000000 ) ) ;
#9857 = ORIENTED_EDGE ( 'NONE', *, *, #2209, .F. ) ;
#9858 = AXIS2_PLACEMENT_3D ( 'NONE', #5566, #10503, #10613 ) ;
#9859 = LINE ( 'NONE', #17016, #1958 ) ;
#9860 = EDGE_CURVE ( 'NONE', #12089, #20860, #12510, .T. ) ;
#9861 = CARTESIAN_POINT ( 'NONE',  ( 84.32438398889955522, -11.28140466348809312, -5.999999999999956479 ) ) ;
#9862 = DIRECTION ( 'NONE',  ( -0.8660254037844384856, 0.000000000000000000, 0.5000000000000003331 ) ) ;
#9863 = CARTESIAN_POINT ( 'NONE',  ( -5.471017171497492448, 36.21317998573887564, -18.88264757256944293 ) ) ;
#9864 = VECTOR ( 'NONE', #3700, 1000.000000000000000 ) ;
#9865 = CARTESIAN_POINT ( 'NONE',  ( 4.630153689607049650, 0.000000000000000000, 0.000000000000000000 ) ) ;
#9866 = DIRECTION ( 'NONE',  ( -1.000000000000000000, 1.276756478318923119E-15, -1.333893503340766797E-15 ) ) ;
#9867 = AXIS2_PLACEMENT_3D ( 'NONE', #9982, #6573, #15375 ) ;
#9868 = CIRCLE ( 'NONE', #16978, 7.000000000000075495 ) ;
#9869 = EDGE_CURVE ( 'NONE', #2652, #22532, #9601, .T. ) ;
#9870 = CARTESIAN_POINT ( 'NONE',  ( -7.909386411296974728, -0.6370970679665923786, 7.731447622712464884 ) ) ;
#9871 = AXIS2_PLACEMENT_3D ( 'NONE', #9855, #1041, #22560 ) ;
#9872 = CARTESIAN_POINT ( 'NONE',  ( 2.499999999999981348, 4.250000000000087041, -17.50000000000001776 ) ) ;
#9873 = CARTESIAN_POINT ( 'NONE',  ( -1.387778780781445676E-14, 2.000000000000001776, -2.000000000000001776 ) ) ;
#9874 = DIRECTION ( 'NONE',  ( 1.550910762415566494E-16, 1.000000000000000000, -8.135128085091684243E-31 ) ) ;
#9875 = CARTESIAN_POINT ( 'NONE',  ( -55.25320565519142946, -4.163336342344337027E-14, 8.000000000000076383 ) ) ;
#9876 = LINE ( 'NONE', #17266, #17502 ) ;
#9877 = VECTOR ( 'NONE', #9554, 1000.000000000000000 ) ;
#9878 = CARTESIAN_POINT ( 'NONE',  ( -2.345747346278134859, 3.264484291692478113, -0.01223254789873211984 ) ) ;
#9879 = ORIENTED_EDGE ( 'NONE', *, *, #2261, .F. ) ;
#9880 = EDGE_CURVE ( 'NONE', #145, #19937, #16754, .T. ) ;
#9881 = VECTOR ( 'NONE', #15523, 1000.000000000000000 ) ;
#9882 = EDGE_LOOP ( 'NONE', ( #511, #11333, #11288, #17072 ) ) ;
#9883 = VECTOR ( 'NONE', #15000, 1000.000000000000227 ) ;
#9884 = AXIS2_PLACEMENT_3D ( 'NONE', #18653, #13718, #20669 ) ;
#9885 = VECTOR ( 'NONE', #17659, 1000.000000000000000 ) ;
#9887 = ORIENTED_EDGE ( 'NONE', *, *, #5663, .F. ) ;
#9886 = ORIENTED_EDGE ( 'NONE', *, *, #7761, .T. ) ;
#9888 = CARTESIAN_POINT ( 'NONE',  ( -6.000000000000047073, -4.800000000000006040, 8.000000000000090594 ) ) ;
#9889 = CARTESIAN_POINT ( 'NONE',  ( -55.25320565519148630, -0.5000000000000281997, 7.500000000000007105 ) ) ;
#9890 = DIRECTION ( 'NONE',  ( 0.000000000000000000, 0.000000000000000000, 1.000000000000000000 ) ) ;
#9891 = CARTESIAN_POINT ( 'NONE',  ( 59.19834661797869302, 0.4999999999999449329, 6.000000000000165201 ) ) ;
#9892 = CYLINDRICAL_SURFACE ( 'NONE', #10550, 2.550000000000003819 ) ;
#9893 = LINE ( 'NONE', #1082, #9881 ) ;
#9894 = CARTESIAN_POINT ( 'NONE',  ( -64.00000000000045475, -7.632783294297951215E-14, -2.000000000000001776 ) ) ;
#9895 = CARTESIAN_POINT ( 'NONE',  ( -7.499999999999992895, -5.999999999999987566, 6.249999999999992006 ) ) ;
#9896 = AXIS2_PLACEMENT_3D ( 'NONE', #18933, #12076, #11864 ) ;
#9897 = FACE_OUTER_BOUND ( 'NONE', #17244, .T. ) ;
#9898 = AXIS2_PLACEMENT_3D ( 'NONE', #12876, #19715, #5600 ) ;
#9899 = DIRECTION ( 'NONE',  ( -0.000000000000000000, -0.000000000000000000, 1.000000000000000000 ) ) ;
#9900 = VECTOR ( 'NONE', #21189, 1000.000000000000114 ) ;
#9901 = CYLINDRICAL_SURFACE ( 'NONE', #2727, 0.5000000000000037748 ) ;
#9902 = AXIS2_PLACEMENT_3D ( 'NONE', #1222, #6740, #1560 ) ;
#9903 = CARTESIAN_POINT ( 'NONE',  ( 63.19496167919713514, -3.291091657286332683, -5.999999999999998224 ) ) ;
#9904 = AXIS2_PLACEMENT_3D ( 'NONE', #20250, #7657, #11521 ) ;
#9905 = AXIS2_PLACEMENT_3D ( 'NONE', #15048, #2356, #20487 ) ;
#9906 = DIRECTION ( 'NONE',  ( 1.000000000000000000, -1.276756478318922922E-15, 1.333893503340766994E-15 ) ) ;
#9907 = CARTESIAN_POINT ( 'NONE',  ( 2.775557561562891351E-14, 8.000000000000003553, -12.50000000000001066 ) ) ;
#9908 = CARTESIAN_POINT ( 'NONE',  ( 0.000000000000000000, 7.999999999999983125, 0.000000000000000000 ) ) ;
#9909 = EDGE_LOOP ( 'NONE', ( #4429, #4811, #1911, #2058, #18850, #4841, #20535 ) ) ;
#9910 = EDGE_CURVE ( 'NONE', #16865, #16772, #10061, .T. ) ;
#9911 = SURFACE_SIDE_STYLE ('',( #16939 ) ) ;
#9913 = ORIENTED_EDGE ( 'NONE', *, *, #4970, .T. ) ;
#9912 = ORIENTED_EDGE ( 'NONE', *, *, #21971, .F. ) ;
#9914 = ORIENTED_EDGE ( 'NONE', *, *, #16692, .F. ) ;
#9915 = CIRCLE ( 'NONE', #5789, 5.749999999999992006 ) ;
#9917 = VERTEX_POINT ( 'NONE', #4290 ) ;
#9916 = ORIENTED_EDGE ( 'NONE', *, *, #23063, .F. ) ;
#9918 = AXIS2_PLACEMENT_3D ( 'NONE', #17917, #16362, #8860 ) ;
#9919 = EDGE_LOOP ( 'NONE', ( #3027, #4221, #10722, #7950 ) ) ;
#9920 = DIRECTION ( 'NONE',  ( 1.000000000000000000, 0.000000000000000000, 0.000000000000000000 ) ) ;
#9921 = VECTOR ( 'NONE', #17486, 1000.000000000000000 ) ;
#9922 = CYLINDRICAL_SURFACE ( 'NONE', #11048, 0.4999999999999987232 ) ;
#9923 = EDGE_LOOP ( 'NONE', ( #11468, #20685, #18975, #10000 ) ) ;
#9924 = DIRECTION ( 'NONE',  ( 0.000000000000000000, -1.000000000000000000, 0.000000000000000000 ) ) ;
#9925 = LINE ( 'NONE', #868, #18295 ) ;
#9926 = LINE ( 'NONE', #4266, #18782 ) ;
#9927 = CARTESIAN_POINT ( 'NONE',  ( -7.854293383767849690, -2.312270958411835498, 7.820081954006687042 ) ) ;
#9928 = PLANE ( 'NONE',  #14810 ) ;
#9929 = CARTESIAN_POINT ( 'NONE',  ( 3.999999999999976463, -0.8732470631450403031, -3.223155494240571795 ) ) ;
#9930 = CARTESIAN_POINT ( 'NONE',  ( 2.681483223904248980, -3.070647092368468112, -5.599999999999979217 ) ) ;
#9931 = CARTESIAN_POINT ( 'NONE',  ( 3.958491816110303319, 1.406739583089060774, 3.499999999999996003 ) ) ;
#9932 = FACE_OUTER_BOUND ( 'NONE', #12262, .T. ) ;
#9933 = DIRECTION ( 'NONE',  ( -2.220446049250313081E-16, 1.000000000000000000, -7.025792437124636392E-31 ) ) ;
#9934 = CIRCLE ( 'NONE', #19710, 0.5000000000000017764 ) ;
#9935 = AXIS2_PLACEMENT_3D ( 'NONE', #16933, #16581, #15181 ) ;
#9936 = CARTESIAN_POINT ( 'NONE',  ( 0.000000000000000000, 0.000000000000000000, -3.499999999999996003 ) ) ;
#9937 = CARTESIAN_POINT ( 'NONE',  ( -5.945013150601167418, 13.92153864138982300, -28.29267684501254010 ) ) ;
#9938 = FACE_OUTER_BOUND ( 'NONE', #18196, .T. ) ;
#9939 = CIRCLE ( 'NONE', #5431, 7.200000000000046363 ) ;
#9940 = EDGE_LOOP ( 'NONE', ( #9366, #686, #7589, #11312, #17042 ) ) ;
#9941 = EDGE_CURVE ( 'NONE', #18303, #21697, #17225, .T. ) ;
#9942 =( NAMED_UNIT ( * ) SI_UNIT ( $, .STERADIAN. ) SOLID_ANGLE_UNIT ( ) );
#9944 = EDGE_LOOP ( 'NONE', ( #6237, #11428 ) ) ;
#9943 = ORIENTED_EDGE ( 'NONE', *, *, #912, .F. ) ;
#9945 = ORIENTED_EDGE ( 'NONE', *, *, #21471, .T. ) ;
#9946 = EDGE_CURVE ( 'NONE', #16059, #1495, #14766, .T. ) ;
#9947 = ORIENTED_EDGE ( 'NONE', *, *, #2109, .F. ) ;
#9948 = EDGE_CURVE ( 'NONE', #18911, #8641, #16995, .T. ) ;
#9949 = ORIENTED_EDGE ( 'NONE', *, *, #16944, .F. ) ;
#9950 = EDGE_CURVE ( 'NONE', #19389, #4887, #3120, .T. ) ;
#9951 = ORIENTED_EDGE ( 'NONE', *, *, #8046, .F. ) ;
#9952 = DIRECTION ( 'NONE',  ( -9.693647360340828445E-26, 0.000000000000000000, 1.000000000000000000 ) ) ;
#9953 = AXIS2_PLACEMENT_3D ( 'NONE', #12584, #19769, #3649 ) ;
#9954 = DIRECTION ( 'NONE',  ( -2.586960666708589311E-16, 0.5000000000000008882, 0.8660254037844381525 ) ) ;
#9955 = ORIENTED_EDGE ( 'NONE', *, *, #761, .F. ) ;
#9956 = FACE_OUTER_BOUND ( 'NONE', #176, .T. ) ;
#9957 = CARTESIAN_POINT ( 'NONE',  ( 1.110223024625156540E-13, 1.749999999999998002, -4.750000000000000888 ) ) ;
#9958 = CARTESIAN_POINT ( 'NONE',  ( 4.165266963751721008, 2.049631966911937830, 3.550066703508936605 ) ) ;
#9959 = CARTESIAN_POINT ( 'NONE',  ( 3.333333333333291737, 2.694301256218282870, -3.300726591567082924 ) ) ;
#9960 = CARTESIAN_POINT ( 'NONE',  ( 80.15235153779141797, -8.074585193523137860, -6.500000000000019540 ) ) ;
#9961 = CARTESIAN_POINT ( 'NONE',  ( 12.84999999999997300, -12.00000000000002842, 5.750000000000018652 ) ) ;
#9962 = EDGE_CURVE ( 'NONE', #11848, #12207, #4760, .T. ) ;
#9963 = CARTESIAN_POINT ( 'NONE',  ( -8.721922330811601398, -13.98762810781391686, 6.818491697976370780 ) ) ;
#9964 = EDGE_CURVE ( 'NONE', #2238, #15768, #4219, .T. ) ;
#9965 = DIRECTION ( 'NONE',  ( -1.613696256722611405E-16, 0.000000000000000000, 1.000000000000000000 ) ) ;
#9966 = CARTESIAN_POINT ( 'NONE',  ( -1.757169849079045659E-15, 3.202582148906729653, 1.452965002680431050 ) ) ;
#9967 = DIRECTION ( 'NONE',  ( 0.000000000000000000, -1.000000000000000000, 0.000000000000000000 ) ) ;
#9968 = ORIENTED_EDGE ( 'NONE', *, *, #484, .F. ) ;
#9969 = EDGE_CURVE ( 'NONE', #16222, #18640, #4528, .T. ) ;
#9970 = CARTESIAN_POINT ( 'NONE',  ( 3.878096787214414753, 3.381939201670116635, 1.142309474598441232 ) ) ;
#9971 = CARTESIAN_POINT ( 'NONE',  ( 2.499999999999981348, 4.250000000000087041, -17.75000000000001776 ) ) ;
#9972 = ORIENTED_EDGE ( 'NONE', *, *, #8923, .T. ) ;
#9973 = ADVANCED_FACE ( 'NONE', ( #20544 ), #15223, .F. ) ;
#9974 = ADVANCED_FACE ( 'NONE', ( #11929 ), #2420, .F. ) ;
#9975 = VERTEX_POINT ( 'NONE', #18887 ) ;
#9976 = EDGE_LOOP ( 'NONE', ( #17125, #11632, #11688, #9272 ) ) ;
#9977 = ADVANCED_FACE ( 'NONE', ( #11467 ), #117, .F. ) ;
#9978 = FACE_OUTER_BOUND ( 'NONE', #2386, .T. ) ;
#9979 = DIRECTION ( 'NONE',  ( -1.454462294001240516E-30, -1.000000000000000000, -0.000000000000000000 ) ) ;
#9980 =( BOUNDED_SURFACE ( )  B_SPLINE_SURFACE ( 3, 2, ( 
 ( #12925, #3858, #233 ),
 ( #19983, #1863, #9402 ),
 ( #10808, #18226, #7518 ),
 ( #9280, #19873, #1750 ),
 ( #20103, #11156, #12575 ),
 ( #3976, #3745, #3641 ) ),
 .UNSPECIFIED., .F., .F., .F. ) 
 B_SPLINE_SURFACE_WITH_KNOTS ( ( 4, 2, 4 ),
 ( 3, 3 ),
 ( 0.01651999345535505245, 0.01858032176739835006, 0.02064065007944164420 ),
 ( 0.000000000000000000, 1.000000000000000000 ),
 .UNSPECIFIED. ) 
 GEOMETRIC_REPRESENTATION_ITEM ( )  RATIONAL_B_SPLINE_SURFACE ( (
 ( 1.000000000000000000, 0.8047781103519392465, 1.000000000000000000),
 ( 1.000000000000000000, 0.8123785825599156851, 1.000000000000000000),
 ( 1.000000000000000000, 0.8190671539795181255, 1.000000000000000000),
 ( 1.000000000000000000, 0.8192352254827984792, 1.000000000000000000),
 ( 1.000000000000000000, 0.8126129677216777925, 1.000000000000000000),
 ( 1.000000000000000000, 0.8047712537969735624, 1.000000000000000000) ) ) 
 REPRESENTATION_ITEM ( '' )  SURFACE ( )  );
#9981 = ORIENTED_EDGE ( 'NONE', *, *, #20987, .F. ) ;
#9982 = CARTESIAN_POINT ( 'NONE',  ( 12.49999999999992362, 1.250000000000015099, -9.500000000000001776 ) ) ;
#9983 = DIRECTION ( 'NONE',  ( -1.000000000000000000, 0.000000000000000000, 0.000000000000000000 ) ) ;
#9984 = DIRECTION ( 'NONE',  ( -0.7071067811865457964, 0.7071067811865492381, 0.000000000000000000 ) ) ;
#9985 = AXIS2_PLACEMENT_3D ( 'NONE', #19872, #3531, #14112 ) ;
#9986 = DIRECTION ( 'NONE',  ( -1.000000000000000000, 1.550910762415566494E-16, 6.133276141584333908E-48 ) ) ;
#9987 = DIRECTION ( 'NONE',  ( -0.7071067811865492381, -0.7071067811865457964, 0.000000000000000000 ) ) ;
#9988 = DIRECTION ( 'NONE',  ( 0.000000000000000000, 0.000000000000000000, 1.000000000000000000 ) ) ;
#9989 = EDGE_CURVE ( 'NONE', #9677, #2242, #14378, .T. ) ;
#9990 = DIRECTION ( 'NONE',  ( 0.2405376366294273427, 0.000000000000000000, -0.9706398123736372785 ) ) ;
#9991 = EDGE_CURVE ( 'NONE', #16222, #22909, #5756, .T. ) ;
#9992 = DIRECTION ( 'NONE',  ( 3.469446951953611428E-15, -1.000000000000000000, 3.469446951953610245E-15 ) ) ;
#9993 = CIRCLE ( 'NONE', #22767, 2.055000000000002380 ) ;
#9994 = PLANE ( 'NONE',  #15887 ) ;
#9995 = CARTESIAN_POINT ( 'NONE',  ( 2.999999999999999556, 9.183364406541944790E-15, -2.500000000000000444 ) ) ;
#9996 = DIRECTION ( 'NONE',  ( 0.000000000000000000, -1.000000000000000000, 0.000000000000000000 ) ) ;
#9997 = FACE_OUTER_BOUND ( 'NONE', #20010, .T. ) ;
#9998 = EDGE_LOOP ( 'NONE', ( #10489, #12127, #18698, #10710 ) ) ;
#9999 = ADVANCED_FACE ( 'NONE', ( #19349 ), #3245, .T. ) ;
#10000 = ORIENTED_EDGE ( 'NONE', *, *, #6635, .F. ) ;
#10002 = EDGE_LOOP ( 'NONE', ( #15792, #10652, #5264, #11639, #10992 ) ) ;
#10001 = ORIENTED_EDGE ( 'NONE', *, *, #2900, .T. ) ;
#10003 = VECTOR ( 'NONE', #9627, 1000.000000000000000 ) ;
#10004 = PLANE ( 'NONE',  #5027 ) ;
#10005 = DIRECTION ( 'NONE',  ( 0.000000000000000000, 0.000000000000000000, -1.000000000000000000 ) ) ;
#10006 = CIRCLE ( 'NONE', #23170, 6.249999999999992006 ) ;
#10007 = CARTESIAN_POINT ( 'NONE',  ( -64.00000000000045475, -7.632783294297951215E-14, -2.000000000000001776 ) ) ;
#10008 = VERTEX_POINT ( 'NONE', #6648 ) ;
#10009 = CARTESIAN_POINT ( 'NONE',  ( 0.000000000000000000, 1.750000000000001554, 0.000000000000000000 ) ) ;
#10010 = CARTESIAN_POINT ( 'NONE',  ( -6.938893903907228378E-14, 4.999999999999976907, -4.163336342344337027E-14 ) ) ;
#10011 = DIRECTION ( 'NONE',  ( 0.000000000000000000, 0.000000000000000000, 1.000000000000000000 ) ) ;
#10012 = CARTESIAN_POINT ( 'NONE',  ( -0.6937372685066998113, 4.453844082567709250, -3.610536846335886008 ) ) ;
#10013 = DIRECTION ( 'NONE',  ( -1.000000000000000000, 0.000000000000000000, 0.000000000000000000 ) ) ;
#10014 = CARTESIAN_POINT ( 'NONE',  ( 0.3126073911696447549, 4.041451884327362798, -2.081668171172168513E-14 ) ) ;
#10015 = FACE_OUTER_BOUND ( 'NONE', #4600, .T. ) ;
#10016 = CARTESIAN_POINT ( 'NONE',  ( 2.249999999999996003, 2.703192042327442355E-14, 17.49999999999997513 ) ) ;
#10017 = DIRECTION ( 'NONE',  ( -0.6819983600624989206, -0.7313537016191700157, 0.000000000000000000 ) ) ;
#10018 = EDGE_CURVE ( 'NONE', #4783, #12739, #19771, .T. ) ;
#10019 = AXIS2_PLACEMENT_3D ( 'NONE', #19735, #22920, #14085 ) ;
#10020 = CYLINDRICAL_SURFACE ( 'NONE', #11564, 0.4999999999999978351 ) ;
#10021 = DIRECTION ( 'NONE',  ( -1.000000000000000000, 0.000000000000000000, 0.000000000000000000 ) ) ;
#10022 = CARTESIAN_POINT ( 'NONE',  ( 54.42435809754118736, 2.499999999999946709, -6.499999999999922728 ) ) ;
#10023 = EDGE_CURVE ( 'NONE', #20684, #774, #1580, .T. ) ;
#10024 = ORIENTED_EDGE ( 'NONE', *, *, #16690, .F. ) ;
#10025 = CIRCLE ( 'NONE', #22413, 0.4999999999999998335 ) ;
#10027 = ORIENTED_EDGE ( 'NONE', *, *, #22163, .T. ) ;
#10026 = VERTEX_POINT ( 'NONE', #17825 ) ;
#10028 = EDGE_CURVE ( 'NONE', #9570, #6059, #7999, .T. ) ;
#10030 = ORIENTED_EDGE ( 'NONE', *, *, #15869, .F. ) ;
#10029 = EDGE_LOOP ( 'NONE', ( #9422, #18703, #7835, #20048 ) ) ;
#10031 = FACE_OUTER_BOUND ( 'NONE', #17420, .T. ) ;
#10032 = CARTESIAN_POINT ( 'NONE',  ( 36.00000000029184832, 2.999999999003851503, -45.00000000000000000 ) ) ;
#10033 = DIRECTION ( 'NONE',  ( -1.000000000000000000, 0.000000000000000000, 0.000000000000000000 ) ) ;
#10034 = AXIS2_PLACEMENT_3D ( 'NONE', #7807, #22160, #15077 ) ;
#10035 = DIRECTION ( 'NONE',  ( 1.000000000000000000, 6.224605580259554159E-31, -2.887593071917436153E-31 ) ) ;
#10036 = CARTESIAN_POINT ( 'NONE',  ( -6.000000000000130562, 7.499999999999958256, -8.000000000000035527 ) ) ;
#10037 = CARTESIAN_POINT ( 'NONE',  ( -8.697224362267958142, -1.999999999999988010, 6.249999999999968914 ) ) ;
#10038 = CIRCLE ( 'NONE', #18299, 4.750000000000013323 ) ;
#10039 = CARTESIAN_POINT ( 'NONE',  ( 3.973110223767139626, -2.262956479381524922E-11, -3.565797985667441328 ) ) ;
#10040 = CARTESIAN_POINT ( 'NONE',  ( -95.20000000000064233, 2.700000000000014833, 1.000000000000014655 ) ) ;
#10041 = CARTESIAN_POINT ( 'NONE',  ( 7.802869476033482243, -2.356467536663165330, 7.917139222843119661 ) ) ;
#10042 = DIRECTION ( 'NONE',  ( -0.9878135252003120703, -1.079983486989479408E-15, 0.1556420233463082226 ) ) ;
#10043 = CARTESIAN_POINT ( 'NONE',  ( 5.599999999999994316, 0.000000000000000000, 0.000000000000000000 ) ) ;
#10044 = CARTESIAN_POINT ( 'NONE',  ( 2.918498775983380256E-10, 2.999999999003851503, -5.999999999999998224 ) ) ;
#10045 = VECTOR ( 'NONE', #13866, 1000.000000000000000 ) ;
#10046 = CARTESIAN_POINT ( 'NONE',  ( -50.65685424949277404, -1.040834085586084257E-13, -7.500000000000062172 ) ) ;
#10047 = PLANE ( 'NONE',  #22093 ) ;
#10048 = CARTESIAN_POINT ( 'NONE',  ( 3.974167765203683089, 0.7238254970432166369, -3.565825589389269190 ) ) ;
#10049 = PRODUCT_DEFINITION_SHAPE ( 'NONE', 'NONE',  #20122 ) ;
#10050 = ORIENTED_EDGE ( 'NONE', *, *, #20890, .T. ) ;
#10051 = CIRCLE ( 'NONE', #7418, 7.200000000000046363 ) ;
#10053 = VERTEX_POINT ( 'NONE', #6761 ) ;
#10052 = ORIENTED_EDGE ( 'NONE', *, *, #19971, .F. ) ;
#10054 = AXIS2_PLACEMENT_3D ( 'NONE', #12415, #8784, #14075 ) ;
#10055 = ORIENTED_EDGE ( 'NONE', *, *, #7654, .F. ) ;
#10056 = ORIENTED_EDGE ( 'NONE', *, *, #10118, .F. ) ;
#10057 = AXIS2_PLACEMENT_3D ( 'NONE', #16620, #9355, #12999 ) ;
#10058 = ORIENTED_EDGE ( 'NONE', *, *, #1681, .F. ) ;
#10059 = CARTESIAN_POINT ( 'NONE',  ( -95.20000000000052864, -3.200000000000064126, 1.000000000000000888 ) ) ;
#10060 = AXIS2_PLACEMENT_3D ( 'NONE', #14275, #21688, #18263 ) ;
#10061 = LINE ( 'NONE', #11824, #20397 ) ;
#10062 = ORIENTED_EDGE ( 'NONE', *, *, #19894, .T. ) ;
#10063 = ORIENTED_EDGE ( 'NONE', *, *, #12634, .T. ) ;
#10064 = CARTESIAN_POINT ( 'NONE',  ( -42.54314575050799618, 3.999999999999996447, 8.000000000000035527 ) ) ;
#10065 = AXIS2_PLACEMENT_3D ( 'NONE', #11912, #6519, #4856 ) ;
#10066 = DIRECTION ( 'NONE',  ( 1.000000000000000000, -1.276756478318923119E-15, 1.387778780781436998E-15 ) ) ;
#10067 = EDGE_CURVE ( 'NONE', #14576, #5046, #6880, .T. ) ;
#10068 = DIRECTION ( 'NONE',  ( 1.066788928082016908E-26, -6.656013887802287108E-31, -1.000000000000000000 ) ) ;
#10069 = FACE_OUTER_BOUND ( 'NONE', #23123, .T. ) ;
#10070 = CARTESIAN_POINT ( 'NONE',  ( -65.00000000000052580, 5.551115123125782702E-14, 3.000000000000002665 ) ) ;
#10071 = DIRECTION ( 'NONE',  ( -1.613696256722611405E-16, 0.000000000000000000, -1.000000000000000000 ) ) ;
#10072 = CIRCLE ( 'NONE', #7823, 2.800000000000017142 ) ;
#10073 = DIRECTION ( 'NONE',  ( -2.013525853228507892E-32, -6.902532920683810383E-31, 1.000000000000000000 ) ) ;
#10074 = CARTESIAN_POINT ( 'NONE',  ( -50.65685424949277404, 3.200000000000022382, 8.000000000000021316 ) ) ;
#10075 = EDGE_CURVE ( 'NONE', #20271, #15092, #9131, .T. ) ;
#10076 = DIRECTION ( 'NONE',  ( 0.000000000000000000, 1.000000000000000000, -0.000000000000000000 ) ) ;
#10077 = VECTOR ( 'NONE', #19614, 1000.000000000000000 ) ;
#10078 = DIRECTION ( 'NONE',  ( 1.000000000000000000, 0.000000000000000000, 0.000000000000000000 ) ) ;
#10079 = EDGE_LOOP ( 'NONE', ( #12337, #12880, #17159, #22714, #4490, #16380, #13736, #12825 ) ) ;
#10080 = MECHANICAL_DESIGN_GEOMETRIC_PRESENTATION_REPRESENTATION (  '', ( #7812 ), #20230 ) ;
#10081 =( NAMED_UNIT ( * ) SI_UNIT ( $, .STERADIAN. ) SOLID_ANGLE_UNIT ( ) );
#10082 = FACE_OUTER_BOUND ( 'NONE', #22793, .T. ) ;
#10083 = AXIS2_PLACEMENT_3D ( 'NONE', #1088, #4717, #11886 ) ;
#10084 = DIRECTION ( 'NONE',  ( 0.000000000000000000, 0.000000000000000000, 1.000000000000000000 ) ) ;
#10085 = VECTOR ( 'NONE', #10177, 1000.000000000000000 ) ;
#10086 = EDGE_LOOP ( 'NONE', ( #4890, #13825, #7008 ) ) ;
#10087 = ORIENTED_EDGE ( 'NONE', *, *, #20199, .F. ) ;
#10088 = EDGE_LOOP ( 'NONE', ( #6166, #8381, #11720 ) ) ;
#10089 = ORIENTED_EDGE ( 'NONE', *, *, #15414, .T. ) ;
#10090 = FACE_OUTER_BOUND ( 'NONE', #21670, .T. ) ;
#10091 = EDGE_CURVE ( 'NONE', #5077, #477, #11378, .T. ) ;
#10092 = CARTESIAN_POINT ( 'NONE',  ( -6.495190528383335327, 5.000000000000018652, -3.750000000000003553 ) ) ;
#10093 = ORIENTED_EDGE ( 'NONE', *, *, #78, .T. ) ;
#10094 = CYLINDRICAL_SURFACE ( 'NONE', #8369, 0.4999999999999995559 ) ;
#10095 = DIRECTION ( 'NONE',  ( 1.000000000000000000, -0.000000000000000000, 0.000000000000000000 ) ) ;
#10096 = DIRECTION ( 'NONE',  ( 0.000000000000000000, 0.000000000000000000, 1.000000000000000000 ) ) ;
#10097 = ADVANCED_FACE ( 'NONE', ( #15919 ), #23128, .T. ) ;
#10098 = AXIS2_PLACEMENT_3D ( 'NONE', #17868, #10563, #17741 ) ;
#10099 = CARTESIAN_POINT ( 'NONE',  ( -5.311293330718551253, 35.99999999900384751, -19.06129441391418666 ) ) ;
#10100 = CARTESIAN_POINT ( 'NONE',  ( -3.499999999708153453, 13.99999999900385106, -19.00000000000000355 ) ) ;
#10101 = AXIS2_PLACEMENT_3D ( 'NONE', #15805, #23133, #7017 ) ;
#10102 = CARTESIAN_POINT ( 'NONE',  ( -7.613388670473234754, -0.8883455870200124282, 8.423574099071704069 ) ) ;
#10103 = DIRECTION ( 'NONE',  ( -1.000000000000000000, 4.615739097524200579E-16, 1.134196829589820086E-15 ) ) ;
#10104 = FACE_OUTER_BOUND ( 'NONE', #14884, .T. ) ;
#10105 = EDGE_CURVE ( 'NONE', #21109, #11093, #12115, .T. ) ;
#10106 = ADVANCED_FACE ( 'NONE', ( #15581, #21122 ), #5355, .T. ) ;
#10107 = CARTESIAN_POINT ( 'NONE',  ( -55.05572809000122447, -3.200000000000088107, -10.00000000000006395 ) ) ;
#10108 = DIRECTION ( 'NONE',  ( 0.000000000000000000, 0.000000000000000000, 1.000000000000000000 ) ) ;
#10109 = CARTESIAN_POINT ( 'NONE',  ( -6.938893903907228378E-15, 1.500000000000001332, 0.000000000000000000 ) ) ;
#10110 = FACE_OUTER_BOUND ( 'NONE', #5375, .T. ) ;
#10111 = B_SPLINE_CURVE_WITH_KNOTS ( 'NONE', 3,
 ( #18600, #6017, #18370, #13421, #15174, #8009, #22368, #20131 ),
 .UNSPECIFIED., .F., .F.,
 ( 4, 2, 2, 4 ),
 ( 0.005324102488572167793, 0.005718019702363091698, 0.006111936916154015603, 0.006899771343735862546 ),
 .UNSPECIFIED. ) ;
#10112 = VERTEX_POINT ( 'NONE', #12161 ) ;
#10113 = CIRCLE ( 'NONE', #20259, 2.500000000000006661 ) ;
#10114 = AXIS2_PLACEMENT_3D ( 'NONE', #21259, #15934, #7143 ) ;
#10115 = AXIS2_PLACEMENT_3D ( 'NONE', #16069, #8800, #9401 ) ;
#10116 = VERTEX_POINT ( 'NONE', #21247 ) ;
#10117 = ADVANCED_FACE ( 'NONE', ( #14294 ), #5243, .T. ) ;
#10118 = EDGE_CURVE ( 'NONE', #6272, #226, #20025, .T. ) ;
#10119 = EDGE_CURVE ( 'NONE', #19838, #5921, #23042, .T. ) ;
#10121 = ORIENTED_EDGE ( 'NONE', *, *, #11836, .T. ) ;
#10120 = ORIENTED_EDGE ( 'NONE', *, *, #18293, .F. ) ;
#10122 = DIRECTION ( 'NONE',  ( -1.000000000000000000, -2.312964634635752325E-16, 1.880120159248731926E-30 ) ) ;
#10123 = DIRECTION ( 'NONE',  ( 9.121204216617949000E-31, 1.000000000000000000, -6.982962677686261977E-15 ) ) ;
#10124 = DIRECTION ( 'NONE',  ( -1.000000000000000000, 0.000000000000000000, 0.000000000000000000 ) ) ;
#10125 = VERTEX_POINT ( 'NONE', #3125 ) ;
#10126 = CARTESIAN_POINT ( 'NONE',  ( -50.65685424949278826, 1.387778780781445676E-14, -7.500000000000034639 ) ) ;
#10127 = ADVANCED_FACE ( 'NONE', ( #19580 ), #21004, .T. ) ;
#10128 = CYLINDRICAL_SURFACE ( 'NONE', #1175, 0.4999999999999995559 ) ;
#10129 = DIRECTION ( 'NONE',  ( 0.000000000000000000, -6.938893903907186568E-15, 1.000000000000000000 ) ) ;
#10130 = DIRECTION ( 'NONE',  ( -1.733449886265891589E-32, 4.190823558986610327E-31, -1.000000000000000000 ) ) ;
#10131 = EDGE_CURVE ( 'NONE', #11666, #2382, #17814, .T. ) ;
#10132 = DIRECTION ( 'NONE',  ( 1.001543066815839268E-16, 2.211965978239706699E-27, 1.000000000000000000 ) ) ;
#10133 = DIRECTION ( 'NONE',  ( 0.7071067811865457964, -0.7071067811865492381, 0.000000000000000000 ) ) ;
#10134 = LINE ( 'NONE', #15298, #16036 ) ;
#10135 = DIRECTION ( 'NONE',  ( -1.000000000000000000, 1.550910762415526064E-16, 0.000000000000000000 ) ) ;
#10136 = PRESENTATION_LAYER_ASSIGNMENT (  '', '', ( #18020 ) ) ;
#10137 = DIRECTION ( 'NONE',  ( -1.000000000000000000, -3.254448077276381206E-32, -1.066788928082016908E-26 ) ) ;
#10138 = PRODUCT_DEFINITION_FORMATION_WITH_SPECIFIED_SOURCE ( 'ANY', '', #6869, .NOT_KNOWN. ) ;
#10139 = VERTEX_POINT ( 'NONE', #12753 ) ;
#10140 = CARTESIAN_POINT ( 'NONE',  ( -80.49101408091227938, 33.72907581769371888, 27.16570243528386186 ) ) ;
#10142 = ORIENTED_EDGE ( 'NONE', *, *, #19019, .T. ) ;
#10141 = VERTEX_POINT ( 'NONE', #18061 ) ;
#10143 = ORIENTED_EDGE ( 'NONE', *, *, #15233, .F. ) ;
#10145 = ORIENTED_EDGE ( 'NONE', *, *, #21054, .F. ) ;
#10144 = VERTEX_POINT ( 'NONE', #12631 ) ;
#10146 = VERTEX_POINT ( 'NONE', #21940 ) ;
#10147 = DIRECTION ( 'NONE',  ( -1.000000000000000000, 1.424116703980815236E-16, 2.931272055834072749E-32 ) ) ;
#10148 = CARTESIAN_POINT ( 'NONE',  ( 3.000000000000002665, 0.000000000000000000, 0.000000000000000000 ) ) ;
#10149 = CIRCLE ( 'NONE', #15764, 5.500000000000046185 ) ;
#10150 = CARTESIAN_POINT ( 'NONE',  ( 4.211140560182139225, 2.431303136016540911, -3.745885042887430405 ) ) ;
#10151 = CARTESIAN_POINT ( 'NONE',  ( 61.48996577904083694, -5.119475911334187224, 6.500000000000130562 ) ) ;
#10152 = CARTESIAN_POINT ( 'NONE',  ( -7.835522544085302243, -2.050824327339882736, 6.894286109559143227 ) ) ;
#10153 = LINE ( 'NONE', #15437, #18948 ) ;
#10154 = DIRECTION ( 'NONE',  ( -2.220446049250313081E-16, 1.000000000000000000, -7.025792437124636392E-31 ) ) ;
#10155 = CARTESIAN_POINT ( 'NONE',  ( 7.568091547083615644, -2.695633093450964246, 8.516664522245834590 ) ) ;
#10156 = CARTESIAN_POINT ( 'NONE',  ( -4.000000000000087041, -2.309401076758553550, -0.5000000000000004441 ) ) ;
#10157 = CARTESIAN_POINT ( 'NONE',  ( -12.84999999999999964, -2.000000000000001776, 5.750000000000005329 ) ) ;
#10158 = EDGE_CURVE ( 'NONE', #20601, #14402, #4986, .T. ) ;
#10159 = CARTESIAN_POINT ( 'NONE',  ( -55.05572809000125289, 2.700000000000021938, -10.00000000000006395 ) ) ;
#10160 = CARTESIAN_POINT ( 'NONE',  ( 66.26395429947841365, -7.000000000000006217, 6.500000000000075495 ) ) ;
#10161 = CARTESIAN_POINT ( 'NONE',  ( -6.979783269036460069, 14.00008466144083030, -26.40130824240443275 ) ) ;
#10162 = CARTESIAN_POINT ( 'NONE',  ( 3.948111298834961591, -0.6968132764971709525, -3.499999999999851230 ) ) ;
#10163 = ORIENTED_EDGE ( 'NONE', *, *, #4200, .T. ) ;
#10164 = AXIS2_PLACEMENT_3D ( 'NONE', #14145, #8733, #6852 ) ;
#10166 = ORIENTED_EDGE ( 'NONE', *, *, #7816, .T. ) ;
#10165 = ORIENTED_EDGE ( 'NONE', *, *, #19941, .T. ) ;
#10167 = ORIENTED_EDGE ( 'NONE', *, *, #7084, .T. ) ;
#10168 = ORIENTED_EDGE ( 'NONE', *, *, #4941, .T. ) ;
#10169 = ORIENTED_EDGE ( 'NONE', *, *, #6951, .T. ) ;
#10170 = VERTEX_POINT ( 'NONE', #12869 ) ;
#10171 = FACE_OUTER_BOUND ( 'NONE', #3797, .T. ) ;
#10172 = DIRECTION ( 'NONE',  ( 1.281898970984144184E-30, 1.000000000000000000, 6.938893903907263876E-15 ) ) ;
#10173 = VERTEX_POINT ( 'NONE', #3807 ) ;
#10174 = CARTESIAN_POINT ( 'NONE',  ( 0.02944718078429346339, -0.6813962075686514908, -3.500000000000035971 ) ) ;
#10175 = DIRECTION ( 'NONE',  ( -3.204747427460357394E-31, 0.8660254037844378194, -0.5000000000000016653 ) ) ;
#10176 = DIRECTION ( 'NONE',  ( -1.756300210255732376E-61, 4.190823558986625216E-31, 1.000000000000000000 ) ) ;
#10177 = DIRECTION ( 'NONE',  ( 3.885780586188016830E-16, 4.437342591868156373E-31, -1.000000000000000000 ) ) ;
#10178 = AXIS2_PLACEMENT_3D ( 'NONE', #21069, #19063, #23189 ) ;
#10179 = DIRECTION ( 'NONE',  ( -1.000000000000000000, 7.477632011778292156E-48, -3.885780586188017323E-16 ) ) ;
#10180 = CARTESIAN_POINT ( 'NONE',  ( 57.49335071782236639, -0.7089083427137543580, -5.999999999999887201 ) ) ;
#10181 = LINE ( 'NONE', #8653, #8692 ) ;
#10182 = CARTESIAN_POINT ( 'NONE',  ( 0.000000000000000000, 0.000000000000000000, 0.000000000000000000 ) ) ;
#10183 = DIRECTION ( 'NONE',  ( 3.254448077146059901E-32, 1.000000000000000000, -6.656013887802287108E-31 ) ) ;
#10184 = CARTESIAN_POINT ( 'NONE',  ( 37.77870956205668307, 4.228348986099717415E-15, -10.69139372032708124 ) ) ;
#10185 = ORIENTED_EDGE ( 'NONE', *, *, #5772, .F. ) ;
#10186 = CARTESIAN_POINT ( 'NONE',  ( -50.65685424949274562, 2.700000000000021938, -8.000000000000062172 ) ) ;
#10187 = ORIENTED_EDGE ( 'NONE', *, *, #12164, .T. ) ;
#10188 = EDGE_CURVE ( 'NONE', #7568, #10218, #15872, .T. ) ;
#10189 = EDGE_LOOP ( 'NONE', ( #21809, #4896, #12589 ) ) ;
#10190 = AXIS2_PLACEMENT_3D ( 'NONE', #18928, #11386, #21159 ) ;
#10191 = MECHANICAL_DESIGN_GEOMETRIC_PRESENTATION_REPRESENTATION (  '', ( #13579 ), #11682 ) ;
#10192 = EDGE_LOOP ( 'NONE', ( #21443, #4361, #8874, #3534 ) ) ;
#10193 = EDGE_LOOP ( 'NONE', ( #2289, #10312, #14505, #21889 ) ) ;
#10194 = VERTEX_POINT ( 'NONE', #20053 ) ;
#10195 = CARTESIAN_POINT ( 'NONE',  ( 4.170895651974849017, 2.054890354522667106, 3.559174498016339339 ) ) ;
#10196 = CYLINDRICAL_SURFACE ( 'NONE', #18192, 0.5000000000000038858 ) ;
#10197 = ORIENTED_EDGE ( 'NONE', *, *, #13389, .T. ) ;
#10198 = CARTESIAN_POINT ( 'NONE',  ( 4.175813232069142344, 4.122719923832743660, 0.000000000000000000 ) ) ;
#10199 = CARTESIAN_POINT ( 'NONE',  ( -67.28510754798014659, -3.200000000000105427, 12.22107821754958579 ) ) ;
#10200 = CARTESIAN_POINT ( 'NONE',  ( -42.54314575050793934, 7.999999999999992895, 7.500000000000062172 ) ) ;
#10201 = LINE ( 'NONE', #20694, #6161 ) ;
#10202 = CARTESIAN_POINT ( 'NONE',  ( 3.972066048304726316, 3.435565134476395333, 1.180968096049722194 ) ) ;
#10203 = CARTESIAN_POINT ( 'NONE',  ( -8.429621201837308675, 1.266960025302491611E-14, 6.425428529985098614 ) ) ;
#10204 = FACE_OUTER_BOUND ( 'NONE', #8998, .T. ) ;
#10205 = DIRECTION ( 'NONE',  ( 1.000000000000000000, -2.168404344971005170E-16, 1.203141491611682442E-30 ) ) ;
#10206 = AXIS2_PLACEMENT_3D ( 'NONE', #7554, #12841, #16702 ) ;
#10207 = AXIS2_PLACEMENT_3D ( 'NONE', #16440, #1554, #7519 ) ;
#10208 = FACE_OUTER_BOUND ( 'NONE', #20686, .T. ) ;
#10209 = DIRECTION ( 'NONE',  ( -1.000000000000000000, -4.440892098500626162E-16, 5.551115123125782702E-16 ) ) ;
#10210 = FACE_BOUND ( 'NONE', #1916, .T. ) ;
#10211 = EDGE_CURVE ( 'NONE', #11574, #8147, #12514, .T. ) ;
#10212 = CARTESIAN_POINT ( 'NONE',  ( 6.500000000000283329, 3.000000000000141220, -5.999999999999943157 ) ) ;
#10213 = ORIENTED_EDGE ( 'NONE', *, *, #3881, .T. ) ;
#10214 = EDGE_CURVE ( 'NONE', #7485, #21952, #21907, .T. ) ;
#10215 = VERTEX_POINT ( 'NONE', #16609 ) ;
#10218 = VERTEX_POINT ( 'NONE', #3697 ) ;
#10217 = EDGE_CURVE ( 'NONE', #21173, #749, #11752, .T. ) ;
#10216 = VERTEX_POINT ( 'NONE', #2155 ) ;
#10219 = AXIS2_PLACEMENT_3D ( 'NONE', #17581, #8187, #1017 ) ;
#10220 = ADVANCED_FACE ( 'NONE', ( #11221 ), #11096, .T. ) ;
#10221 = CYLINDRICAL_SURFACE ( 'NONE', #8020, 6.500000000000023981 ) ;
#10222 = CIRCLE ( 'NONE', #13237, 2.549999999999997158 ) ;
#10223 = EDGE_CURVE ( 'NONE', #20271, #8929, #14420, .T. ) ;
#10224 = VECTOR ( 'NONE', #12549, 1000.000000000000114 ) ;
#10225 = CARTESIAN_POINT ( 'NONE',  ( 42.50000000000014921, 8.000000000000003553, -14.99999999999998579 ) ) ;
#10226 = CARTESIAN_POINT ( 'NONE',  ( 4.113620667976075396, -1.749999999999998002, -2.375000000000002220 ) ) ;
#10227 = EDGE_LOOP ( 'NONE', ( #2585, #21300, #18022, #17456 ) ) ;
#10228 = FACE_OUTER_BOUND ( 'NONE', #14622, .T. ) ;
#10229 = CARTESIAN_POINT ( 'NONE',  ( 4.071447262713891568, -2.020725942163709377, -3.499999999999999556 ) ) ;
#10230 = DIRECTION ( 'NONE',  ( -5.551115123561405253E-17, -1.000000000000000000, -2.256980353643891447E-27 ) ) ;
#10231 = CARTESIAN_POINT ( 'NONE',  ( 2.918498775983380256E-10, 2.999999999003851503, -12.99999999999999822 ) ) ;
#10232 = PRESENTATION_LAYER_ASSIGNMENT (  '', '', ( #6872 ) ) ;
#10233 = CARTESIAN_POINT ( 'NONE',  ( 119.5756419024615269, -4.000000000000003553, 6.500000000000123457 ) ) ;
#10234 = LINE ( 'NONE', #10016, #6117 ) ;
#10235 = CARTESIAN_POINT ( 'NONE',  ( -3.806930669195367489, 0.7500000000000509592, -3.000000000000000444 ) ) ;
#10236 = EDGE_CURVE ( 'NONE', #10905, #22731, #4877, .T. ) ;
#10237 = CARTESIAN_POINT ( 'NONE',  ( -89.70000000000057128, -0.5000000000000628386, -2.000000000000001776 ) ) ;
#10238 = AXIS2_PLACEMENT_3D ( 'NONE', #14412, #12277, #9113 ) ;
#10239 = CARTESIAN_POINT ( 'NONE',  ( 4.175813232069142344, -4.122719923832743660, 0.000000000000000000 ) ) ;
#10240 = AXIS2_PLACEMENT_3D ( 'NONE', #784, #6423, #9954 ) ;
#10241 = AXIS2_PLACEMENT_3D ( 'NONE', #1139, #15227, #6312 ) ;
#10242 = VERTEX_POINT ( 'NONE', #5830 ) ;
#10243 = VECTOR ( 'NONE', #4087, 1000.000000000000000 ) ;
#10244 = CARTESIAN_POINT ( 'NONE',  ( -68.59459193786533149, 38.58681605307294404, 22.16570243528389028 ) ) ;
#10246 = ORIENTED_EDGE ( 'NONE', *, *, #11116, .F. ) ;
#10245 = ORIENTED_EDGE ( 'NONE', *, *, #18447, .T. ) ;
#10247 = UNCERTAINTY_MEASURE_WITH_UNIT (LENGTH_MEASURE( 1.000000000000000082E-05 ), #7825, 'distance_accuracy_value', 'NONE');
#10248 = APPLICATION_CONTEXT ( 'automotive_design' ) ;
#10249 = ADVANCED_FACE ( 'NONE', ( #12990 ), #3589, .T. ) ;
#10250 = ORIENTED_EDGE ( 'NONE', *, *, #2439, .T. ) ;
#10253 = ORIENTED_EDGE ( 'NONE', *, *, #21581, .T. ) ;
#10252 = ADVANCED_FACE ( 'NONE', ( #6712 ), #9529, .T. ) ;
#10251 = ORIENTED_EDGE ( 'NONE', *, *, #11153, .T. ) ;
#10254 = ORIENTED_EDGE ( 'NONE', *, *, #12245, .F. ) ;
#10255 = DIRECTION ( 'NONE',  ( 0.000000000000000000, 1.000000000000000000, 0.000000000000000000 ) ) ;
#10256 = EDGE_CURVE ( 'NONE', #9446, #4139, #17406, .T. ) ;
#10257 = PLANE ( 'NONE',  #9583 ) ;
#10258 = DIRECTION ( 'NONE',  ( -5.546678239835239257E-32, -1.000000000000000000, 6.938893903907215756E-15 ) ) ;
#10259 = AXIS2_PLACEMENT_3D ( 'NONE', #14789, #18432, #18213 ) ;
#10260 = TOROIDAL_SURFACE ( 'NONE', #4611, 5.500000000000003553, 0.5000000000000000000 ) ;
#10261 = DIRECTION ( 'NONE',  ( -5.551115123561405253E-17, -1.000000000000000000, -2.256980353643891447E-27 ) ) ;
#10262 = AXIS2_PLACEMENT_3D ( 'NONE', #12099, #11990, #6596 ) ;
#10263 = DIRECTION ( 'NONE',  ( -2.220446049250313081E-16, 1.000000000000000000, -7.025792437124636392E-31 ) ) ;
#10264 = DIRECTION ( 'NONE',  ( 0.000000000000000000, -1.000000000000000000, 0.000000000000000000 ) ) ;
#10265 = AXIS2_PLACEMENT_3D ( 'NONE', #1551, #10598, #14488 ) ;
#10266 = CARTESIAN_POINT ( 'NONE',  ( 3.951447005078448260, -1.347150628109125226, 3.499999999999996891 ) ) ;
#10267 = CARTESIAN_POINT ( 'NONE',  ( 24.75000000000000355, 2.000000000000029310, -3.469446951953614189E-15 ) ) ;
#10268 = CARTESIAN_POINT ( 'NONE',  ( 42.00000000000014921, 2.999999999999999112, 2.500000000000030198 ) ) ;
#10269 = DIRECTION ( 'NONE',  ( -1.000000000000000000, -4.440892098500626162E-16, 5.551115123125782702E-16 ) ) ;
#10270 = CARTESIAN_POINT ( 'NONE',  ( -4.000000000000003553, 0.000000000000000000, 0.000000000000000000 ) ) ;
#10271 = CARTESIAN_POINT ( 'NONE',  ( -3.499999999708153453, 38.99999999900385461, -26.50000000000000000 ) ) ;
#10272 = CARTESIAN_POINT ( 'NONE',  ( -4.000000000000104805, 0.8730739991738779571, -3.223134629628646941 ) ) ;
#10273 = CARTESIAN_POINT ( 'NONE',  ( 4.180345304246195326, -2.049116244671344678, 3.591763845239302366 ) ) ;
#10274 = EDGE_LOOP ( 'NONE', ( #6876, #17242, #13817, #3240 ) ) ;
#10275 = VECTOR ( 'NONE', #21260, 1000.000000000000114 ) ;
#10276 = AXIS2_PLACEMENT_3D ( 'NONE', #14922, #5653, #7870 ) ;
#10278 = ORIENTED_EDGE ( 'NONE', *, *, #17147, .F. ) ;
#10277 = EDGE_LOOP ( 'NONE', ( #16402, #1352, #3029, #12183 ) ) ;
#10279 = AXIS2_PLACEMENT_3D ( 'NONE', #814, #1051, #9986 ) ;
#10280 = ADVANCED_FACE ( 'NONE', ( #3189 ), #13339, .T. ) ;
#10281 = CIRCLE ( 'NONE', #7665, 6.249999999999992006 ) ;
#10282 = AXIS2_PLACEMENT_3D ( 'NONE', #14110, #8936, #8 ) ;
#10283 = ORIENTED_EDGE ( 'NONE', *, *, #924, .T. ) ;
#10284 = EDGE_LOOP ( 'NONE', ( #6590, #21241, #14468, #6818 ) ) ;
#10285 = EDGE_LOOP ( 'NONE', ( #15218, #18616, #13926, #14992, #7350 ) ) ;
#10286 = ORIENTED_EDGE ( 'NONE', *, *, #16090, .T. ) ;
#10287 = CARTESIAN_POINT ( 'NONE',  ( 4.690415759823415520, 0.7500000000000700551, -2.000000000000001776 ) ) ;
#10288 = DIRECTION ( 'NONE',  ( 0.000000000000000000, -6.938893903907237055E-15, -1.000000000000000000 ) ) ;
#10289 = EDGE_LOOP ( 'NONE', ( #16723, #10698, #21862, #19729, #6183 ) ) ;
#10290 = FACE_OUTER_BOUND ( 'NONE', #524, .T. ) ;
#10291 = DIRECTION ( 'NONE',  ( -1.550910762415566494E-16, -1.000000000000000000, 8.135128085091684243E-31 ) ) ;
#10292 = TOROIDAL_SURFACE ( 'NONE', #21948, 3.500000000000001776, 0.5000000000000000000 ) ;
#10293 = FACE_OUTER_BOUND ( 'NONE', #19949, .T. ) ;
#10294 = AXIS2_PLACEMENT_3D ( 'NONE', #12250, #6993, #8739 ) ;
#10295 = CARTESIAN_POINT ( 'NONE',  ( 4.071447262713891568, -4.041451884327432076, 1.040834085586084257E-14 ) ) ;
#10296 = DIRECTION ( 'NONE',  ( -1.232595164407830946E-32, 1.000000000000000000, -6.938893903907214967E-15 ) ) ;
#10297 = DIRECTION ( 'NONE',  ( 3.330669073875432643E-16, 4.437342591868153746E-31, -1.000000000000000000 ) ) ;
#10298 = VECTOR ( 'NONE', #2278, 1000.000000000000000 ) ;
#10299 = DIRECTION ( 'NONE',  ( -1.000000000000000000, 1.276756478318923119E-15, -1.403805528459192781E-15 ) ) ;
#10300 = FILL_AREA_STYLE_COLOUR ( '', #19213 ) ;
#10301 = LINE ( 'NONE', #8434, #15729 ) ;
#10302 = CARTESIAN_POINT ( 'NONE',  ( -4.733938537004360292, 13.62597557122357372, -16.08514644908176905 ) ) ;
#10303 = DIRECTION ( 'NONE',  ( 1.000000000000000000, -4.190823558986610327E-31, 1.733449886265890494E-32 ) ) ;
#10304 = ORIENTED_EDGE ( 'NONE', *, *, #19029, .T. ) ;
#10305 = DIRECTION ( 'NONE',  ( -0.000000000000000000, 0.000000000000000000, -1.000000000000000000 ) ) ;
#10306 = DIRECTION ( 'NONE',  ( 0.000000000000000000, 0.000000000000000000, 1.000000000000000000 ) ) ;
#10308 = ORIENTED_EDGE ( 'NONE', *, *, #18153, .F. ) ;
#10307 = VERTEX_POINT ( 'NONE', #757 ) ;
#10309 = ADVANCED_FACE ( 'NONE', ( #10228 ), #1188, .F. ) ;
#10310 = AXIS2_PLACEMENT_3D ( 'NONE', #9080, #12247, #23106 ) ;
#10311 = ADVANCED_BREP_SHAPE_REPRESENTATION ( '', ( #20673, #22115 ), #2988 ) ;
#10312 = ORIENTED_EDGE ( 'NONE', *, *, #16981, .T. ) ;
#10313 = AXIS2_PLACEMENT_3D ( 'NONE', #8150, #15317, #18624 ) ;
#10314 = VECTOR ( 'NONE', #9225, 1000.000000000000000 ) ;
#10315 = EDGE_CURVE ( 'NONE', #19106, #6591, #5931, .T. ) ;
#10316 = ORIENTED_EDGE ( 'NONE', *, *, #13713, .F. ) ;
#10317 = CARTESIAN_POINT ( 'NONE',  ( 4.142654963991854622, 2.035398498734347417, 3.525413613457306639 ) ) ;
#10318 = CARTESIAN_POINT ( 'NONE',  ( 2.775557561562891351E-14, 0.4999999999999726885, -6.000000000000019540 ) ) ;
#10319 = DIRECTION ( 'NONE',  ( -0.7313537016191734574, 0.6819983600624954789, -3.733258675956565293E-18 ) ) ;
#10320 = CARTESIAN_POINT ( 'NONE',  ( 4.180231891692618440, 4.134807952925578789, 0.02076457676760740112 ) ) ;
#10321 = DIRECTION ( 'NONE',  ( -9.121204216617949000E-31, -1.000000000000000000, 6.982962677686261977E-15 ) ) ;
#10322 = FACE_OUTER_BOUND ( 'NONE', #15654, .T. ) ;
#10323 = DIRECTION ( 'NONE',  ( -0.7313537016191746787, -0.6819983600624940356, -1.072890437865584409E-16 ) ) ;
#10324 = CARTESIAN_POINT ( 'NONE',  ( -6.999999995197900837, -0.7826352830280864925, 9.233045673661063546 ) ) ;
#10325 = ADVANCED_FACE ( 'NONE', ( #21067 ), #6530, .T. ) ;
#10326 = DIRECTION ( 'NONE',  ( -1.550910762415566494E-16, -1.000000000000000000, 8.135128085091684243E-31 ) ) ;
#10327 = VECTOR ( 'NONE', #8710, 1000.000000000000114 ) ;
#10328 = DIRECTION ( 'NONE',  ( 0.7071067811865490160, 0.7071067811865460184, 1.565905175853766674E-16 ) ) ;
#10329 = AXIS2_PLACEMENT_3D ( 'NONE', #14490, #11291, #4115 ) ;
#10330 = CARTESIAN_POINT ( 'NONE',  ( 7.500000000000007105, -5.999999999999981348, 11.74999999999995559 ) ) ;
#10331 = CARTESIAN_POINT ( 'NONE',  ( -1.387778780781445676E-14, -8.271819572847247670, 0.000000000000000000 ) ) ;
#10332 = CARTESIAN_POINT ( 'NONE',  ( -45.91923881554277642, -2.462384566050232593, 8.000000000000047962 ) ) ;
#10333 = CARTESIAN_POINT ( 'NONE',  ( -2.855764796983377263, 2.970025579236395874, -0.09382832055445512742 ) ) ;
#10334 = ORIENTED_EDGE ( 'NONE', *, *, #9120, .F. ) ;
#10335 = ORIENTED_EDGE ( 'NONE', *, *, #16432, .F. ) ;
#10336 = CARTESIAN_POINT ( 'NONE',  ( -1.734723475976807094E-14, 2.000000000000001776, -17.00000000000000711 ) ) ;
#10338 = ORIENTED_EDGE ( 'NONE', *, *, #4921, .F. ) ;
#10337 = ORIENTED_EDGE ( 'NONE', *, *, #22725, .T. ) ;
#10339 = AXIS2_PLACEMENT_3D ( 'NONE', #21063, #6948, #22951 ) ;
#10340 = DIRECTION ( 'NONE',  ( 1.454462294001240516E-30, 1.000000000000000000, 0.000000000000000000 ) ) ;
#10341 = EDGE_LOOP ( 'NONE', ( #13065, #20772, #15068, #9449 ) ) ;
#10342 = DIRECTION ( 'NONE',  ( 3.032184104443271834E-30, 1.000000000000000000, 4.437342591868167759E-31 ) ) ;
#10343 = PRODUCT_RELATED_PRODUCT_CATEGORY ( 'part', '', ( #4976 ) ) ;
#10344 = DIRECTION ( 'NONE',  ( -1.000000000000000000, 1.389842848855773367E-62, -2.013525853228507892E-32 ) ) ;
#10345 = ORIENTED_EDGE ( 'NONE', *, *, #23239, .T. ) ;
#10346 = DIRECTION ( 'NONE',  ( -1.331202777560457422E-30, -1.000000000000000000, 7.395570986446985676E-31 ) ) ;
#10347 = CARTESIAN_POINT ( 'NONE',  ( 27.99999999999991473, -3.469446951953614189E-15, -2.775557561562891351E-14 ) ) ;
#10348 = DIRECTION ( 'NONE',  ( 1.454462294001240516E-30, 1.000000000000000000, 0.000000000000000000 ) ) ;
#10349 = CARTESIAN_POINT ( 'NONE',  ( 4.000000000000003553, -0.3902508023145569993, -1.999844788467403101E-15 ) ) ;
#10350 = ADVANCED_FACE ( 'NONE', ( #22273 ), #13104, .F. ) ;
#10351 = CARTESIAN_POINT ( 'NONE',  ( 30.60000000000000142, 2.800724053285369664E-14, -2.055000000000020144 ) ) ;
#10352 = TOROIDAL_SURFACE ( 'NONE', #9606, 2.250000000000000444, 0.2500000000000000000 ) ;
#10353 = CARTESIAN_POINT ( 'NONE',  ( 0.000000000000000000, 1.750000000000001554, 0.000000000000000000 ) ) ;
#10354 = CARTESIAN_POINT ( 'NONE',  ( -45.01801948466091829, 6.474873734152911453, -7.500000000000062172 ) ) ;
#10355 = SURFACE_SIDE_STYLE ('',( #19300 ) ) ;
#10356 = EDGE_CURVE ( 'NONE', #283, #5825, #20520, .T. ) ;
#10357 = FACE_BOUND ( 'NONE', #20123, .T. ) ;
#10358 = EDGE_CURVE ( 'NONE', #5921, #7127, #1307, .T. ) ;
#10359 = VERTEX_POINT ( 'NONE', #20396 ) ;
#10360 = AXIS2_PLACEMENT_3D ( 'NONE', #4612, #17430, #4735 ) ;
#10361 = DIRECTION ( 'NONE',  ( 5.551115123125765446E-17, -3.053113317719182458E-16, -1.000000000000000000 ) ) ;
#10363 = ORIENTED_EDGE ( 'NONE', *, *, #3328, .F. ) ;
#10362 = EDGE_LOOP ( 'NONE', ( #6788, #5107, #1778, #21784 ) ) ;
#10364 = CIRCLE ( 'NONE', #8122, 0.5000000000000000000 ) ;
#10365 = VERTEX_POINT ( 'NONE', #22161 ) ;
#10367 = VERTEX_POINT ( 'NONE', #13770 ) ;
#10366 = ORIENTED_EDGE ( 'NONE', *, *, #23149, .F. ) ;
#10368 = ORIENTED_EDGE ( 'NONE', *, *, #2484, .T. ) ;
#10369 = CARTESIAN_POINT ( 'NONE',  ( -4.000000000000002665, 1.557668341133494838, -0.1596965656957533841 ) ) ;
#10370 = LINE ( 'NONE', #10720, #19732 ) ;
#10371 = EDGE_CURVE ( 'NONE', #12394, #1148, #9146, .T. ) ;
#10372 = PLANE ( 'NONE',  #20051 ) ;
#10373 = CARTESIAN_POINT ( 'NONE',  ( 1.999999999999953149, -3.464101615137771262, 0.000000000000000000 ) ) ;
#10374 = AXIS2_PLACEMENT_3D ( 'NONE', #9032, #16186, #102 ) ;
#10375 = CARTESIAN_POINT ( 'NONE',  ( -3.499999999708153453, 35.49999999900384751, -26.00000000000000000 ) ) ;
#10376 = FACE_OUTER_BOUND ( 'NONE', #14, .T. ) ;
#10377 = DIRECTION ( 'NONE',  ( -7.860214984770699307E-18, 1.409037165336591006E-16, 1.000000000000000000 ) ) ;
#10378 = ADVANCED_FACE ( 'NONE', ( #13214 ), #11560, .F. ) ;
#10379 = DIRECTION ( 'NONE',  ( 0.000000000000000000, 0.000000000000000000, 1.000000000000000000 ) ) ;
#10380 = FACE_OUTER_BOUND ( 'NONE', #23093, .T. ) ;
#10381 = CARTESIAN_POINT ( 'NONE',  ( 4.086376210449940594, 2.103254844323305228, 3.499999999999968026 ) ) ;
#10382 = DIRECTION ( 'NONE',  ( 0.000000000000000000, 0.000000000000000000, -1.000000000000000000 ) ) ;
#10383 = AXIS2_PLACEMENT_3D ( 'NONE', #3599, #19238, #22903 ) ;
#10384 = CARTESIAN_POINT ( 'NONE',  ( 2.775557561562891351E-14, 8.000000000000003553, -6.499999999999950262 ) ) ;
#10385 = ADVANCED_FACE ( 'NONE', ( #4148 ), #16263, .F. ) ;
#10386 = DIRECTION ( 'NONE',  ( 0.000000000000000000, -6.938893903907237844E-15, -1.000000000000000000 ) ) ;
#10387 = EDGE_CURVE ( 'NONE', #23176, #18843, #3875, .T. ) ;
#10388 = AXIS2_PLACEMENT_3D ( 'NONE', #12967, #12733, #21913 ) ;
#10389 = CARTESIAN_POINT ( 'NONE',  ( -4.211399284164375700, 2.459729995988197526, -3.751162237960563139 ) ) ;
#10390 = CARTESIAN_POINT ( 'NONE',  ( 8.660254037844344666, -2.775557561562891351E-14, 2.081668171172168513E-14 ) ) ;
#10391 = VERTEX_POINT ( 'NONE', #9578 ) ;
#10393 = ORIENTED_EDGE ( 'NONE', *, *, #8232, .F. ) ;
#10392 = ORIENTED_EDGE ( 'NONE', *, *, #22201, .T. ) ;
#10394 = EDGE_LOOP ( 'NONE', ( #786, #12181, #1456, #16539 ) ) ;
#10395 = CIRCLE ( 'NONE', #10019, 2.550000000000024691 ) ;
#10396 = VERTEX_POINT ( 'NONE', #4264 ) ;
#10398 = ORIENTED_EDGE ( 'NONE', *, *, #18187, .T. ) ;
#10397 = EDGE_CURVE ( 'NONE', #17574, #4163, #18349, .T. ) ;
#10399 = ADVANCED_FACE ( 'NONE', ( #11441 ), #12454, .T. ) ;
#10400 = AXIS2_PLACEMENT_3D ( 'NONE', #19102, #17210, #8289 ) ;
#10401 = VERTEX_POINT ( 'NONE', #3644 ) ;
#10402 = EDGE_CURVE ( 'NONE', #10662, #23066, #18003, .T. ) ;
#10403 = CARTESIAN_POINT ( 'NONE',  ( -6.938893903907228378E-14, 4.999999999999976907, -4.163336342344337027E-14 ) ) ;
#10404 = EDGE_CURVE ( 'NONE', #12740, #22474, #19643, .T. ) ;
#10405 = CIRCLE ( 'NONE', #7781, 5.200000000000008171 ) ;
#10406 = AXIS2_PLACEMENT_3D ( 'NONE', #18830, #8128, #12194 ) ;
#10407 = DIRECTION ( 'NONE',  ( 1.000000000000000000, -4.440892098500651800E-16, -7.860214984771115307E-18 ) ) ;
#10408 = ORIENTED_EDGE ( 'NONE', *, *, #11736, .F. ) ;
#10409 = CARTESIAN_POINT ( 'NONE',  ( -3.345653888883676430, 2.687187980154690958, -0.1391502195351397297 ) ) ;
#10410 = CARTESIAN_POINT ( 'NONE',  ( 12.84999999999998721, -13.50000000000003020, 6.250000000000033751 ) ) ;
#10411 = CIRCLE ( 'NONE', #665, 0.5000000000000029976 ) ;
#10412 = CARTESIAN_POINT ( 'NONE',  ( -2.804994570502229223, -3.229033611042515073, -3.526374918436863126 ) ) ;
#10413 = FACE_OUTER_BOUND ( 'NONE', #21357, .T. ) ;
#10414 = CARTESIAN_POINT ( 'NONE',  ( -7.786490775660069197, -0.7065074219475123707, 7.963863235126036777 ) ) ;
#10415 = CARTESIAN_POINT ( 'NONE',  ( -8.660254037844421049, 4.999999999999948486, -1.387778780781445676E-14 ) ) ;
#10416 = ADVANCED_FACE ( 'NONE', ( #10579 ), #23072, .T. ) ;
#10417 = CARTESIAN_POINT ( 'NONE',  ( -43.46238456605044576, 4.919238815542528620, -8.000000000000035527 ) ) ;
#10418 =( NAMED_UNIT ( * ) SI_UNIT ( $, .STERADIAN. ) SOLID_ANGLE_UNIT ( ) );
#10419 = DIRECTION ( 'NONE',  ( 0.2405376366294550983, 0.000000000000000000, -0.9706398123736303951 ) ) ;
#10420 = EDGE_CURVE ( 'NONE', #20563, #7229, #8270, .T. ) ;
#10421 = DIRECTION ( 'NONE',  ( 1.756300210255732376E-61, -4.190823558986625216E-31, -1.000000000000000000 ) ) ;
#10422 = VECTOR ( 'NONE', #6113, 1000.000000000000114 ) ;
#10423 = DIRECTION ( 'NONE',  ( -1.134196829589822059E-15, -6.741645191078037727E-32, 1.000000000000000000 ) ) ;
#10424 = AXIS2_PLACEMENT_3D ( 'NONE', #11602, #6666, #18790 ) ;
#10425 = ORIENTED_EDGE ( 'NONE', *, *, #3651, .F. ) ;
#10426 = DIRECTION ( 'NONE',  ( -2.013525853228518840E-32, 6.902532920683810383E-31, -1.000000000000000000 ) ) ;
#10427 = DIRECTION ( 'NONE',  ( -2.220446049250313081E-16, 1.000000000000000000, -7.025792437124636392E-31 ) ) ;
#10429 = EDGE_LOOP ( 'NONE', ( #3822, #21238, #8324, #7599 ) ) ;
#10428 = ORIENTED_EDGE ( 'NONE', *, *, #11022, .T. ) ;
#10430 = AXIS2_PLACEMENT_3D ( 'NONE', #10009, #13885, #15757 ) ;
#10431 = VECTOR ( 'NONE', #14722, 1000.000000000000000 ) ;
#10432 = VERTEX_POINT ( 'NONE', #12338 ) ;
#10433 = PRODUCT_DEFINITION_SHAPE ( 'NONE', 'NONE',  #23280 ) ;
#10434 = CIRCLE ( 'NONE', #3308, 0.5000000000000029976 ) ;
#10435 = EDGE_LOOP ( 'NONE', ( #17538, #10777, #2003, #10052 ) ) ;
#10436 = CARTESIAN_POINT ( 'NONE',  ( 77.42435809754137210, -3.999999999999809042, -5.999999999999984901 ) ) ;
#10437 = DIRECTION ( 'NONE',  ( 1.733449886265891589E-32, -4.190823558986610327E-31, 1.000000000000000000 ) ) ;
#10438 = LINE ( 'NONE', #8909, #9110 ) ;
#10439 = CARTESIAN_POINT ( 'NONE',  ( 0.4637351970278864033, -1.750000000000002665, 4.749999999999999112 ) ) ;
#10440 = AXIS2_PLACEMENT_3D ( 'NONE', #507, #7678, #5910 ) ;
#10441 = CARTESIAN_POINT ( 'NONE',  ( 124.5000000000017764, -4.000000000000003553, 6.000000000000116351 ) ) ;
#10442 = CARTESIAN_POINT ( 'NONE',  ( 77.42435809754130105, -10.99999999999981526, 6.000000000000123457 ) ) ;
#10443 = LINE ( 'NONE', #21626, #10077 ) ;
#10444 = CIRCLE ( 'NONE', #3296, 2.000000000000000000 ) ;
#10445 = CARTESIAN_POINT ( 'NONE',  ( -7.500000000000016875, -1.217419751679961415, 9.022398393216642276 ) ) ;
#10446 = ADVANCED_FACE ( 'NONE', ( #19403 ), #12136, .T. ) ;
#10447 = DIRECTION ( 'NONE',  ( 1.066786462891689527E-26, 6.656013887802287108E-31, 1.000000000000000000 ) ) ;
#10448 = CARTESIAN_POINT ( 'NONE',  ( -4.113620667976089607, -1.750000000000001554, -2.375000000000005773 ) ) ;
#10449 = AXIS2_PLACEMENT_3D ( 'NONE', #4106, #20117, #14930 ) ;
#10450 = CARTESIAN_POINT ( 'NONE',  ( -6.999999999708142795, 13.99999999900385106, -19.00000000000000355 ) ) ;
#10451 = DIRECTION ( 'NONE',  ( -0.000000000000000000, 1.000000000000000000, 0.000000000000000000 ) ) ;
#10452 = CARTESIAN_POINT ( 'NONE',  ( 29.00000000029184832, 16.99999999900385461, -26.50000000000000000 ) ) ;
#10453 = ADVANCED_FACE ( 'NONE', ( #3748 ), #5532, .F. ) ;
#10454 = DIRECTION ( 'NONE',  ( -1.000000000000000000, -3.254448077276381206E-32, -1.066788928082016908E-26 ) ) ;
#10455 = DIRECTION ( 'NONE',  ( 0.000000000000000000, 0.000000000000000000, 1.000000000000000000 ) ) ;
#10456 = EDGE_LOOP ( 'NONE', ( #12204, #10368, #18360, #5414 ) ) ;
#10457 = AXIS2_PLACEMENT_3D ( 'NONE', #6382, #13434, #22380 ) ;
#10458 = ORIENTED_EDGE ( 'NONE', *, *, #461, .T. ) ;
#10459 = AXIS2_PLACEMENT_3D ( 'NONE', #17615, #5502, #18086 ) ;
#10460 = CARTESIAN_POINT ( 'NONE',  ( -4.896882909240444448, 36.38534960922712713, -26.01795247534147393 ) ) ;
#10461 = AXIS2_PLACEMENT_3D ( 'NONE', #7963, #21750, #14670 ) ;
#10463 = VERTEX_POINT ( 'NONE', #21302 ) ;
#10462 = VERTEX_POINT ( 'NONE', #8827 ) ;
#10464 = AXIS2_PLACEMENT_3D ( 'NONE', #11280, #16561, #14585 ) ;
#10465 = VECTOR ( 'NONE', #15695, 1000.000000000000000 ) ;
#10466 = CARTESIAN_POINT ( 'NONE',  ( -4.113620667976089607, 1.749999999999998002, -2.375000000000029754 ) ) ;
#10467 = ORIENTED_EDGE ( 'NONE', *, *, #8097, .F. ) ;
#10468 = CARTESIAN_POINT ( 'NONE',  ( 2.855764796983322640, -2.970025579236485136, -0.09382832055448196706 ) ) ;
#10469 = LINE ( 'NONE', #17637, #736 ) ;
#10470 = VERTEX_POINT ( 'NONE', #10471 ) ;
#10471 = CARTESIAN_POINT ( 'NONE',  ( 10.50000000000000888, -12.00000000000002842, 5.750000000000032863 ) ) ;
#10472 = CARTESIAN_POINT ( 'NONE',  ( -9.714451465470119729E-14, 1.999999999999890754, 8.000000000000090594 ) ) ;
#10473 = CARTESIAN_POINT ( 'NONE',  ( 10.50000000000000888, -12.50000000000002842, 6.250000000000061284 ) ) ;
#10474 = PLANE ( 'NONE',  #152 ) ;
#10475 =( GEOMETRIC_REPRESENTATION_CONTEXT ( 3 ) GLOBAL_UNCERTAINTY_ASSIGNED_CONTEXT ( ( #22261 ) ) GLOBAL_UNIT_ASSIGNED_CONTEXT ( ( #4666, #9844, #19025 ) ) REPRESENTATION_CONTEXT ( 'NONE', 'WORKASPACE' ) );
#10476 = DIRECTION ( 'NONE',  ( -1.000000000000000000, 0.000000000000000000, -2.668805347656595124E-16 ) ) ;
#10477 = CARTESIAN_POINT ( 'NONE',  ( 4.132952817037869764, 2.031684012687259955, -3.518979934899760131 ) ) ;
#10478 = VECTOR ( 'NONE', #379, 1000.000000000000000 ) ;
#10479 = CYLINDRICAL_SURFACE ( 'NONE', #9715, 0.5000000000000004441 ) ;
#10480 = MECHANICAL_DESIGN_GEOMETRIC_PRESENTATION_REPRESENTATION (  '', ( #20634 ), #20652 ) ;
#10481 = AXIS2_PLACEMENT_3D ( 'NONE', #11833, #17471, #6772 ) ;
#10482 = VERTEX_POINT ( 'NONE', #3535 ) ;
#10483 = DIRECTION ( 'NONE',  ( 0.3371777511303412633, 0.4730117276049429775, 0.8139846863982593828 ) ) ;
#10485 = ORIENTED_EDGE ( 'NONE', *, *, #3509, .T. ) ;
#10484 = VERTEX_POINT ( 'NONE', #15981 ) ;
#10486 = EDGE_CURVE ( 'NONE', #19482, #21027, #23057, .T. ) ;
#10487 = ORIENTED_EDGE ( 'NONE', *, *, #12959, .T. ) ;
#10489 = ORIENTED_EDGE ( 'NONE', *, *, #18995, .T. ) ;
#10488 = ORIENTED_EDGE ( 'NONE', *, *, #15535, .F. ) ;
#10490 = DIRECTION ( 'NONE',  ( 1.000000000000000000, 4.708535149079844747E-14, 3.717264591378824873E-16 ) ) ;
#10491 = DIRECTION ( 'NONE',  ( 3.330669073875432643E-16, 4.437342591868153746E-31, -1.000000000000000000 ) ) ;
#10492 = DIRECTION ( 'NONE',  ( -1.000000000000000000, -2.699383410053119644E-30, -3.330669073875432643E-16 ) ) ;
#10493 = AXIS2_PLACEMENT_3D ( 'NONE', #12606, #18140, #7107 ) ;
#10494 = FACE_OUTER_BOUND ( 'NONE', #17481, .T. ) ;
#10495 = DIRECTION ( 'NONE',  ( 3.469446951953619316E-15, -6.938893903907238633E-15, -1.000000000000000000 ) ) ;
#10496 = DIRECTION ( 'NONE',  ( -1.000000000000000000, -1.479114197289397135E-31, -5.916456789157588541E-31 ) ) ;
#10497 = DIRECTION ( 'NONE',  ( -3.885780586188016830E-16, -4.437342591868156373E-31, 1.000000000000000000 ) ) ;
#10498 = CARTESIAN_POINT ( 'NONE',  ( 119.5756419024615838, -11.00000000000006573, -6.000000000000116351 ) ) ;
#10499 = CARTESIAN_POINT ( 'NONE',  ( 24.99999999999995737, 2.000000000000001776, -16.99999999999997868 ) ) ;
#10500 = DIRECTION ( 'NONE',  ( -0.7071067811865457964, 0.7071067811865492381, 0.000000000000000000 ) ) ;
#10501 = AXIS2_PLACEMENT_3D ( 'NONE', #19400, #8242, #22712 ) ;
#10502 = CARTESIAN_POINT ( 'NONE',  ( 1.391697335622787080, 4.043246145443402995, -3.503898532754375239 ) ) ;
#10503 = DIRECTION ( 'NONE',  ( -1.000000000000000000, -3.254448077276381206E-32, -1.066788928082016908E-26 ) ) ;
#10504 = AXIS2_PLACEMENT_3D ( 'NONE', #6607, #3080, #14130 ) ;
#10505 = DIRECTION ( 'NONE',  ( -1.550910762415566494E-16, -1.000000000000000000, 8.135128085091684243E-31 ) ) ;
#10506 = FACE_OUTER_BOUND ( 'NONE', #5176, .T. ) ;
#10507 = DIRECTION ( 'NONE',  ( -1.000000000000000000, -2.699383410053118943E-30, -2.668805347656595124E-16 ) ) ;
#10508 = LINE ( 'NONE', #3232, #8525 ) ;
#10509 = ORIENTED_EDGE ( 'NONE', *, *, #5991, .F. ) ;
#10510 = ADVANCED_FACE ( 'NONE', ( #1532 ), #12905, .T. ) ;
#10511 =( NAMED_UNIT ( * ) SI_UNIT ( $, .STERADIAN. ) SOLID_ANGLE_UNIT ( ) );
#10513 = ORIENTED_EDGE ( 'NONE', *, *, #5437, .F. ) ;
#10512 = ORIENTED_EDGE ( 'NONE', *, *, #8442, .F. ) ;
#10514 = ADVANCED_FACE ( 'NONE', ( #5294 ), #2387, .T. ) ;
#10515 = ORIENTED_EDGE ( 'NONE', *, *, #12242, .F. ) ;
#10516 = ORIENTED_EDGE ( 'NONE', *, *, #14197, .T. ) ;
#10517 = VECTOR ( 'NONE', #9579, 1000.000000000000000 ) ;
#10518 = ORIENTED_EDGE ( 'NONE', *, *, #21604, .F. ) ;
#10519 = CIRCLE ( 'NONE', #13122, 3.499999999999999556 ) ;
#10520 = ORIENTED_EDGE ( 'NONE', *, *, #7676, .T. ) ;
#10521 = FACE_OUTER_BOUND ( 'NONE', #8608, .T. ) ;
#10522 = ADVANCED_FACE ( 'NONE', ( #5422 ), #15, .T. ) ;
#10523 = EDGE_CURVE ( 'NONE', #3580, #17187, #13016, .T. ) ;
#10524 = CARTESIAN_POINT ( 'NONE',  ( 0.02944718078671985234, -0.6813962075909525407, 3.499999999999960032 ) ) ;
#10525 = ORIENTED_EDGE ( 'NONE', *, *, #7533, .T. ) ;
#10526 = DIRECTION ( 'NONE',  ( 1.000000000000000000, 2.168404344971017743E-16, -1.780660105995169760E-30 ) ) ;
#10527 = DIRECTION ( 'NONE',  ( 0.000000000000000000, 0.000000000000000000, 1.000000000000000000 ) ) ;
#10528 = CARTESIAN_POINT ( 'NONE',  ( -6.958039891257955745, 36.00029345514013102, -26.50000000000000000 ) ) ;
#10529 = LINE ( 'NONE', #13515, #17015 ) ;
#10530 = CARTESIAN_POINT ( 'NONE',  ( -12.84999999999999964, -2.000000000000001776, 0.000000000000000000 ) ) ;
#10531 = CARTESIAN_POINT ( 'NONE',  ( 36.00000000029184832, 49.99999999900385461, -16.00000000000000000 ) ) ;
#10532 = FACE_OUTER_BOUND ( 'NONE', #15138, .T. ) ;
#10533 = CARTESIAN_POINT ( 'NONE',  ( 4.071447262713891568, 4.041451884327377009, -2.081668171172168513E-14 ) ) ;
#10534 = VECTOR ( 'NONE', #3775, 1000.000000000000000 ) ;
#10535 = CARTESIAN_POINT ( 'NONE',  ( -55.25320565519140104, -2.700000000000049472, 7.500000000000047962 ) ) ;
#10536 = CYLINDRICAL_SURFACE ( 'NONE', #8511, 2.549999999999996714 ) ;
#10537 = EDGE_LOOP ( 'NONE', ( #10428, #4985, #6335, #14734 ) ) ;
#10538 = EDGE_CURVE ( 'NONE', #6361, #8991, #124, .T. ) ;
#10539 =( NAMED_UNIT ( * ) SI_UNIT ( $, .STERADIAN. ) SOLID_ANGLE_UNIT ( ) );
#10540 = CARTESIAN_POINT ( 'NONE',  ( 116.8476484622116232, -8.074585193523331483, 6.500000000000040856 ) ) ;
#10541 = CARTESIAN_POINT ( 'NONE',  ( -4.365918574175958078, 13.48846683486500808, -28.98347793635020864 ) ) ;
#10543 = EDGE_LOOP ( 'NONE', ( #13326, #4785, #7349, #13483 ) ) ;
#10542 = ORIENTED_EDGE ( 'NONE', *, *, #11284, .F. ) ;
#10544 = ORIENTED_EDGE ( 'NONE', *, *, #17515, .T. ) ;
#10546 = ORIENTED_EDGE ( 'NONE', *, *, #7394, .T. ) ;
#10545 = ADVANCED_FACE ( 'NONE', ( #6955 ), #5776, .T. ) ;
#10547 = DIRECTION ( 'NONE',  ( -1.000000000000000000, 0.000000000000000000, -4.336808689941968432E-16 ) ) ;
#10548 = CARTESIAN_POINT ( 'NONE',  ( 0.000000000000000000, 2.999999999999992450, 0.000000000000000000 ) ) ;
#10549 = EDGE_CURVE ( 'NONE', #20921, #21696, #18921, .T. ) ;
#10550 = AXIS2_PLACEMENT_3D ( 'NONE', #20491, #7770, #16928 ) ;
#10551 = CARTESIAN_POINT ( 'NONE',  ( 3.345653888883671989, -2.687187980154742473, -0.1391502195351571880 ) ) ;
#10552 = LINE ( 'NONE', #5144, #21292 ) ;
#10553 = EDGE_CURVE ( 'NONE', #11666, #15881, #22103, .T. ) ;
#10554 = CARTESIAN_POINT ( 'NONE',  ( 2.499999999999960476, 4.250000000000017764, -19.00000000000002132 ) ) ;
#10555 = LINE ( 'NONE', #8799, #9476 ) ;
#10556 = FACE_OUTER_BOUND ( 'NONE', #21983, .T. ) ;
#10557 = FACE_OUTER_BOUND ( 'NONE', #12540, .T. ) ;
#10558 = CARTESIAN_POINT ( 'NONE',  ( -2.805705207896105779, 3.226868319750133107, -3.503898532754362805 ) ) ;
#10559 = DIRECTION ( 'NONE',  ( -0.000000000000000000, 1.000000000000000000, -0.000000000000000000 ) ) ;
#10560 = CARTESIAN_POINT ( 'NONE',  ( 37.60054931026104441, 10.94797865062591669, -10.60054931026143166 ) ) ;
#10561 = DIRECTION ( 'NONE',  ( 0.7313537016191735685, -0.6819983600624951459, 3.923113172947598083E-16 ) ) ;
#10562 = DIRECTION ( 'NONE',  ( 2.710505431213791653E-16, 1.000000000000000000, -4.807121141190541565E-31 ) ) ;
#10563 = DIRECTION ( 'NONE',  ( 0.7313537016191746787, 0.6819983600624940356, 1.072890437865584409E-16 ) ) ;
#10565 = VECTOR ( 'NONE', #9175, 1000.000000000000000 ) ;
#10564 = CARTESIAN_POINT ( 'NONE',  ( 12.84999999999997300, -2.000000000000001776, -6.249999999999992006 ) ) ;
#10566 = VERTEX_POINT ( 'NONE', #7521 ) ;
#10567 = ORIENTED_EDGE ( 'NONE', *, *, #20475, .T. ) ;
#10568 = ORIENTED_EDGE ( 'NONE', *, *, #22338, .T. ) ;
#10569 = ADVANCED_FACE ( 'NONE', ( #5647 ), #21566, .T. ) ;
#10570 = CARTESIAN_POINT ( 'NONE',  ( -6.979889398518855259, 35.99999999900384751, -26.48728129910209006 ) ) ;
#10572 = EDGE_LOOP ( 'NONE', ( #4362, #4402, #804, #12329 ) ) ;
#10571 = ORIENTED_EDGE ( 'NONE', *, *, #22790, .F. ) ;
#10573 = CARTESIAN_POINT ( 'NONE',  ( 3.436319922986410536, -2.634841920959276163, -3.531542292954277240 ) ) ;
#10574 = DIRECTION ( 'NONE',  ( 3.032184104443272185E-30, 1.000000000000000000, -7.395570986447005381E-32 ) ) ;
#10575 = EDGE_CURVE ( 'NONE', #11319, #18271, #17796, .T. ) ;
#10576 = LINE ( 'NONE', #10225, #15961 ) ;
#10577 = CARTESIAN_POINT ( 'NONE',  ( 6.938893903907228378E-15, 4.618802153517023612, -3.433295621305385126 ) ) ;
#10578 = ORIENTED_EDGE ( 'NONE', *, *, #17415, .T. ) ;
#10579 = FACE_OUTER_BOUND ( 'NONE', #4372, .T. ) ;
#10580 = CIRCLE ( 'NONE', #7219, 0.5000000000000028866 ) ;
#10581 = CIRCLE ( 'NONE', #13595, 0.5000000000000006661 ) ;
#10582 = CARTESIAN_POINT ( 'NONE',  ( 0.000000000000000000, 0.000000000000000000, 3.499999999999975131 ) ) ;
#10583 = DIRECTION ( 'NONE',  ( 0.000000000000000000, 0.000000000000000000, 1.000000000000000000 ) ) ;
#10584 = CARTESIAN_POINT ( 'NONE',  ( 4.000000000000004441, -1.549102112939114484, -0.1578953385959453726 ) ) ;
#10585 = CARTESIAN_POINT ( 'NONE',  ( -90.55603112840523750, -2.700000000000084110, -7.432974388601742533 ) ) ;
#10586 = SHAPE_REPRESENTATION ( 'Base', ( #22115 ), #7836 ) ;
#10587 = CARTESIAN_POINT ( 'NONE',  ( 3.999999999999950706, 1.539600717839022082, -3.300726591567077595 ) ) ;
#10588 = DIRECTION ( 'NONE',  ( 1.000000000000000000, -1.424116703980815236E-16, -2.931272055834072749E-32 ) ) ;
#10589 = CARTESIAN_POINT ( 'NONE',  ( -2.700000000000132960, 1.999999999999904521, 8.000000000000076383 ) ) ;
#10590 = CARTESIAN_POINT ( 'NONE',  ( -50.65685424949281668, 3.200000000000022382, -7.500000000000089706 ) ) ;
#10591 = ORIENTED_EDGE ( 'NONE', *, *, #21353, .F. ) ;
#10592 = AXIS2_PLACEMENT_3D ( 'NONE', #1087, #8252, #22373 ) ;
#10594 = EDGE_LOOP ( 'NONE', ( #8295, #20887, #22829, #12157, #19936 ) ) ;
#10593 = EDGE_LOOP ( 'NONE', ( #2762, #16405, #22332, #7453 ) ) ;
#10595 = VERTEX_POINT ( 'NONE', #581 ) ;
#10597 = EDGE_LOOP ( 'NONE', ( #1236, #1005, #6264, #21526 ) ) ;
#10596 = ORIENTED_EDGE ( 'NONE', *, *, #8585, .F. ) ;
#10598 = DIRECTION ( 'NONE',  ( -2.220446049250313081E-16, 1.000000000000000000, -7.025792437124636392E-31 ) ) ;
#10599 = ADVANCED_FACE ( 'NONE', ( #3862 ), #18167, .T. ) ;
#10600 = DIRECTION ( 'NONE',  ( -2.013525853228507892E-32, -6.902532920683810383E-31, 1.000000000000000000 ) ) ;
#10601 = SURFACE_STYLE_FILL_AREA ( #19549 ) ;
#10602 = ORIENTED_EDGE ( 'NONE', *, *, #7246, .F. ) ;
#10603 = DIRECTION ( 'NONE',  ( 0.9706398123736329486, -1.505375731439247187E-16, 0.2405376366294442458 ) ) ;
#10604 = CONICAL_SURFACE ( 'NONE', #13245, 5.371010071662833063, 1.221730476396037490 ) ;
#10605 = CARTESIAN_POINT ( 'NONE',  ( -67.40537636629493079, 2.081668171172168513E-14, 12.70639812373644517 ) ) ;
#10606 = CARTESIAN_POINT ( 'NONE',  ( 7.607945571813336194, -13.10245601331112653, 8.443122311927350410 ) ) ;
#10607 = DIRECTION ( 'NONE',  ( 1.000000000000000000, -3.816391647148972452E-14, 0.000000000000000000 ) ) ;
#10608 = CARTESIAN_POINT ( 'NONE',  ( 3.000000000000002665, 0.000000000000000000, 0.000000000000000000 ) ) ;
#10609 = DIRECTION ( 'NONE',  ( 0.000000000000000000, -0.000000000000000000, 1.000000000000000000 ) ) ;
#10610 = AXIS2_PLACEMENT_3D ( 'NONE', #21007, #19116, #1365 ) ;
#10611 = DIRECTION ( 'NONE',  ( 0.7313537016191730133, -0.6819983600624958120, 5.924440990721418971E-17 ) ) ;
#10612 = CIRCLE ( 'NONE', #9867, 4.750000000000000888 ) ;
#10613 = DIRECTION ( 'NONE',  ( 0.000000000000000000, 0.000000000000000000, 1.000000000000000000 ) ) ;
#10614 = EDGE_CURVE ( 'NONE', #21236, #13097, #9514, .T. ) ;
#10615 = LINE ( 'NONE', #15786, #7818 ) ;
#10616 = EDGE_CURVE ( 'NONE', #1495, #15578, #701, .T. ) ;
#10617 = CARTESIAN_POINT ( 'NONE',  ( 7.491585531133562625, -2.143791077336254514, 7.320610673787141920 ) ) ;
#10618 = CARTESIAN_POINT ( 'NONE',  ( -4.000000000000108358, -2.472261339043379635, -3.687027428081224301 ) ) ;
#10619 = CARTESIAN_POINT ( 'NONE',  ( 4.180231891692618440, -4.134807952925569907, -0.02076457676760569415 ) ) ;
#10620 = PRODUCT_DEFINITION_SHAPE ( 'NONE', 'NONE',  #23285 ) ;
#10621 = ORIENTED_EDGE ( 'NONE', *, *, #22938, .F. ) ;
#10623 = ORIENTED_EDGE ( 'NONE', *, *, #18450, .F. ) ;
#10622 = ORIENTED_EDGE ( 'NONE', *, *, #8682, .T. ) ;
#10624 = ORIENTED_EDGE ( 'NONE', *, *, #17910, .F. ) ;
#10625 = CIRCLE ( 'NONE', #8445, 0.5000000000000004441 ) ;
#10627 = ORIENTED_EDGE ( 'NONE', *, *, #8373, .T. ) ;
#10626 = VERTEX_POINT ( 'NONE', #9285 ) ;
#10628 = AXIS2_PLACEMENT_3D ( 'NONE', #14372, #14494, #19431 ) ;
#10629 = EDGE_LOOP ( 'NONE', ( #14598, #11463, #12215, #21291 ) ) ;
#10630 = STYLED_ITEM ( 'NONE', ( #19817 ), #10220 ) ;
#10631 = AXIS2_PLACEMENT_3D ( 'NONE', #14375, #18142, #5452 ) ;
#10632 = EDGE_LOOP ( 'NONE', ( #17631, #9448, #2695, #18729 ) ) ;
#10633 = AXIS2_PLACEMENT_3D ( 'NONE', #3090, #10255, #19317 ) ;
#10634 = ORIENTED_EDGE ( 'NONE', *, *, #2745, .F. ) ;
#10635 = CARTESIAN_POINT ( 'NONE',  ( 63.50658097017375070, -4.500000000000003553, 6.000000000000185629 ) ) ;
#10636 = CARTESIAN_POINT ( 'NONE',  ( 5.599999999999994316, -2.020725942163695166, -3.500000000000007550 ) ) ;
#10637 = CARTESIAN_POINT ( 'NONE',  ( -4.000000000000003553, 2.309401076758494487, -0.3572655899081629283 ) ) ;
#10638 = DIRECTION ( 'NONE',  ( -8.438582421954109416E-32, 0.000000000000000000, -1.000000000000000000 ) ) ;
#10639 = EDGE_CURVE ( 'NONE', #21725, #16028, #5409, .T. ) ;
#10640 = DIRECTION ( 'NONE',  ( 0.000000000000000000, 3.382522293539643228E-32, 1.000000000000000000 ) ) ;
#10641 = FACE_OUTER_BOUND ( 'NONE', #8557, .T. ) ;
#10642 = DIRECTION ( 'NONE',  ( 0.000000000000000000, 6.938893903907237055E-15, 1.000000000000000000 ) ) ;
#10643 = FILL_AREA_STYLE_COLOUR ( '', #20393 ) ;
#10644 =( LENGTH_UNIT ( ) NAMED_UNIT ( * ) SI_UNIT ( .MILLI., .METRE. ) );
#10645 = CARTESIAN_POINT ( 'NONE',  ( 0.000000000000000000, 0.000000000000000000, 0.000000000000000000 ) ) ;
#10646 = VECTOR ( 'NONE', #9035, 1000.000000000000114 ) ;
#10647 = VECTOR ( 'NONE', #5766, 1000.000000000000000 ) ;
#10648 = CYLINDRICAL_SURFACE ( 'NONE', #10665, 4.000000000000014211 ) ;
#10649 = AXIS2_PLACEMENT_3D ( 'NONE', #5995, #16444, #14684 ) ;
#10650 = CARTESIAN_POINT ( 'NONE',  ( -8.200527591913209235, -1.560621988374211178, 7.318116290495742859 ) ) ;
#10651 = TOROIDAL_SURFACE ( 'NONE', #521, 4.500000000000002665, 0.5000000000000000000 ) ;
#10652 = ORIENTED_EDGE ( 'NONE', *, *, #2987, .T. ) ;
#10653 = AXIS2_PLACEMENT_3D ( 'NONE', #15632, #22823, #13878 ) ;
#10654 = STYLED_ITEM ( 'NONE', ( #17195 ), #12881 ) ;
#10655 = ADVANCED_FACE ( 'NONE', ( #354 ), #11384, .F. ) ;
#10656 = SURFACE_STYLE_USAGE ( .BOTH. , #17597 ) ;
#10657 = CARTESIAN_POINT ( 'NONE',  ( -6.000000000000088818, -2.000000000000043521, -7.500000000000007105 ) ) ;
#10658 = DIRECTION ( 'NONE',  ( 0.5833333333333344806, -8.095376221225076634E-15, -0.8122328620674129640 ) ) ;
#10660 = EDGE_LOOP ( 'NONE', ( #15915, #22651, #15745, #313 ) ) ;
#10659 = ORIENTED_EDGE ( 'NONE', *, *, #6064, .F. ) ;
#10661 = ADVANCED_FACE ( 'NONE', ( #11497 ), #3521, .T. ) ;
#10662 = VERTEX_POINT ( 'NONE', #21870 ) ;
#10663 = ORIENTED_EDGE ( 'NONE', *, *, #15451, .T. ) ;
#10664 = DIRECTION ( 'NONE',  ( -3.254448077146059901E-32, -1.000000000000000000, -6.409494854920712161E-31 ) ) ;
#10665 = AXIS2_PLACEMENT_3D ( 'NONE', #1714, #17705, #7144 ) ;
#10666 = VECTOR ( 'NONE', #534, 1000.000000000000000 ) ;
#10667 = CARTESIAN_POINT ( 'NONE',  ( 8.718376657154808029, -0.4999999999999831246, 6.820622386031985229 ) ) ;
#10668 = CIRCLE ( 'NONE', #3522, 6.000000000000047073 ) ;
#10669 = DIRECTION ( 'NONE',  ( 0.000000000000000000, -3.469446951953622866E-15, -1.000000000000000000 ) ) ;
#10670 = FACE_OUTER_BOUND ( 'NONE', #5951, .T. ) ;
#10671 = EDGE_CURVE ( 'NONE', #11093, #5891, #16333, .T. ) ;
#10672 = EDGE_CURVE ( 'NONE', #8469, #3083, #2011, .T. ) ;
#10673 = DIRECTION ( 'NONE',  ( 1.331202777560457422E-30, 1.000000000000000000, -7.395570986446985676E-31 ) ) ;
#10674 = CARTESIAN_POINT ( 'NONE',  ( -3.499999999708153453, 42.99999999900385461, -19.00000000000000355 ) ) ;
#10675 = CARTESIAN_POINT ( 'NONE',  ( 8.954763739086866181, -12.50000000000002132, 6.678571428571491886 ) ) ;
#10676 = DIRECTION ( 'NONE',  ( -1.000000000000000000, 1.550910762415510534E-16, 0.000000000000000000 ) ) ;
#10677 = EDGE_CURVE ( 'NONE', #21644, #10770, #22314, .T. ) ;
#10678 = DIRECTION ( 'NONE',  ( 1.000000000000000000, 2.168404344970991858E-16, 0.000000000000000000 ) ) ;
#10679 = DIRECTION ( 'NONE',  ( 0.000000000000000000, 1.000000000000000000, 0.000000000000000000 ) ) ;
#10680 = DIRECTION ( 'NONE',  ( 0.000000000000000000, -1.000000000000000000, 0.000000000000000000 ) ) ;
#10681 = DIRECTION ( 'NONE',  ( 1.134196829589819889E-15, -1.111653967262545517E-30, 1.000000000000000000 ) ) ;
#10682 =( NAMED_UNIT ( * ) SI_UNIT ( $, .STERADIAN. ) SOLID_ANGLE_UNIT ( ) );
#10683 = VECTOR ( 'NONE', #2053, 1000.000000000000114 ) ;
#10684 = ADVANCED_FACE ( 'NONE', ( #18571 ), #16671, .T. ) ;
#10685 = AXIS2_PLACEMENT_3D ( 'NONE', #21772, #589, #9293 ) ;
#10686 = CARTESIAN_POINT ( 'NONE',  ( 5.100000000000007638, 0.000000000000000000, 0.000000000000000000 ) ) ;
#10687 = ORIENTED_EDGE ( 'NONE', *, *, #1522, .T. ) ;
#10688 = EDGE_LOOP ( 'NONE', ( #12893, #427, #16876, #14698, #22357, #2176 ) ) ;
#10689 = CARTESIAN_POINT ( 'NONE',  ( -6.130979318138412459, 35.99999999900384751, -26.13052066537846940 ) ) ;
#10691 = ORIENTED_EDGE ( 'NONE', *, *, #16294, .T. ) ;
#10690 = ORIENTED_EDGE ( 'NONE', *, *, #3881, .F. ) ;
#10692 = DIRECTION ( 'NONE',  ( -2.775557561562883647E-17, 3.652049423109057473E-16, -1.000000000000000000 ) ) ;
#10693 = DIRECTION ( 'NONE',  ( 3.885780586188016830E-16, 4.437342591868156373E-31, -1.000000000000000000 ) ) ;
#10694 = ADVANCED_FACE ( 'NONE', ( #4096 ), #7746, .F. ) ;
#10695 = PLANE ( 'NONE',  #12375 ) ;
#10696 = VECTOR ( 'NONE', #10130, 1000.000000000000000 ) ;
#10697 = ADVANCED_FACE ( 'NONE', ( #22695 ), #3891, .T. ) ;
#10698 = ORIENTED_EDGE ( 'NONE', *, *, #368, .T. ) ;
#10699 = DIRECTION ( 'NONE',  ( 1.550910762415566494E-16, 1.000000000000000000, -8.135128085091684243E-31 ) ) ;
#10700 = DIRECTION ( 'NONE',  ( -4.190823558986625216E-31, 1.000000000000000000, -4.190823558986625216E-31 ) ) ;
#10701 = LINE ( 'NONE', #18345, #21830 ) ;
#10702 = FACE_OUTER_BOUND ( 'NONE', #9742, .T. ) ;
#10703 = CARTESIAN_POINT ( 'NONE',  ( 3.973110223765540017, 0.6902454861566492683, -3.565797985667426673 ) ) ;
#10704 = FACE_OUTER_BOUND ( 'NONE', #13474, .T. ) ;
#10705 = CARTESIAN_POINT ( 'NONE',  ( 2.100000000000011635, -2.681188604469753282E-15, -0.2800830152838794107 ) ) ;
#10706 = CARTESIAN_POINT ( 'NONE',  ( 3.961551342854190860, -3.742715940867750835, 0.5174258321191379517 ) ) ;
#10707 = EDGE_CURVE ( 'NONE', #23176, #9421, #6576, .T. ) ;
#10708 = DIRECTION ( 'NONE',  ( -0.000000000000000000, 1.000000000000000000, -0.000000000000000000 ) ) ;
#10709 = CARTESIAN_POINT ( 'NONE',  ( 7.500000000000007105, -11.35410196624971491, 9.250000000000021316 ) ) ;
#10710 = ORIENTED_EDGE ( 'NONE', *, *, #1892, .T. ) ;
#10711 = AXIS2_PLACEMENT_3D ( 'NONE', #4325, #2572, #7988 ) ;
#10712 = PRODUCT_CONTEXT ( 'NONE', #22871, 'mechanical' ) ;
#10713 = VECTOR ( 'NONE', #2948, 1000.000000000000000 ) ;
#10715 = ORIENTED_EDGE ( 'NONE', *, *, #8110, .T. ) ;
#10714 = ORIENTED_EDGE ( 'NONE', *, *, #20170, .T. ) ;
#10716 = ORIENTED_EDGE ( 'NONE', *, *, #22905, .F. ) ;
#10718 = ORIENTED_EDGE ( 'NONE', *, *, #2593, .F. ) ;
#10717 = ORIENTED_EDGE ( 'NONE', *, *, #20136, .F. ) ;
#10719 = CARTESIAN_POINT ( 'NONE',  ( 4.140404888673258732, 2.228338276487474179, -3.686887068327037831 ) ) ;
#10720 = CARTESIAN_POINT ( 'NONE',  ( -0.5000000000000837108, 1.999999999999883871, 8.000000000000076383 ) ) ;
#10721 = CARTESIAN_POINT ( 'NONE',  ( 7.670621117724267357, -11.48840066917087022, 8.215271161873694439 ) ) ;
#10722 = ORIENTED_EDGE ( 'NONE', *, *, #12133, .T. ) ;
#10723 = AXIS2_PLACEMENT_3D ( 'NONE', #12907, #16072, #2076 ) ;
#10724 = CYLINDRICAL_SURFACE ( 'NONE', #12228, 0.5000000000000017764 ) ;
#10725 = CARTESIAN_POINT ( 'NONE',  ( -7.332081355611433260, -0.2267865287842164845, 7.890992604157045065 ) ) ;
#10726 = CARTESIAN_POINT ( 'NONE',  ( 8.137537312224765174, -13.43749107754207017, 7.396067884835384021 ) ) ;
#10727 = ADVANCED_FACE ( 'NONE', ( #12068 ), #6676, .F. ) ;
#10728 = FILL_AREA_STYLE ('',( #16014 ) ) ;
#10729 = FACE_OUTER_BOUND ( 'NONE', #17454, .T. ) ;
#10730 = DIRECTION ( 'NONE',  ( 1.000000000000000000, -1.276756478318922330E-15, 0.000000000000000000 ) ) ;
#10731 = DIRECTION ( 'NONE',  ( -1.733449886265891589E-32, 4.190823558986610327E-31, -1.000000000000000000 ) ) ;
#10732 = APPLICATION_CONTEXT ( 'automotive_design' ) ;
#10733 = DIRECTION ( 'NONE',  ( 0.000000000000000000, 0.000000000000000000, -1.000000000000000000 ) ) ;
#10734 = EDGE_CURVE ( 'NONE', #13735, #13332, #10201, .T. ) ;
#10735 = CARTESIAN_POINT ( 'NONE',  ( 24.99999999999996447, 1.999999999999988010, -18.74999999999998224 ) ) ;
#10736 = CIRCLE ( 'NONE', #15980, 0.4999999999999994449 ) ;
#10737 = CARTESIAN_POINT ( 'NONE',  ( 2.775557561562891351E-14, 5.500000000000001776, -15.49999999999998579 ) ) ;
#10738 = LINE ( 'NONE', #12495, #12309 ) ;
#10739 = CARTESIAN_POINT ( 'NONE',  ( 3.974175853610027342, -3.450041667725643801, 1.156004144283955704 ) ) ;
#10740 = ADVANCED_FACE ( 'NONE', ( #17255 ), #154, .T. ) ;
#10741 = ORIENTED_EDGE ( 'NONE', *, *, #2682, .T. ) ;
#10742 = FILL_AREA_STYLE_COLOUR ( '', #11987 ) ;
#10744 = ORIENTED_EDGE ( 'NONE', *, *, #17685, .T. ) ;
#10743 = ORIENTED_EDGE ( 'NONE', *, *, #17473, .F. ) ;
#10745 = ORIENTED_EDGE ( 'NONE', *, *, #11252, .F. ) ;
#10747 = ORIENTED_EDGE ( 'NONE', *, *, #15249, .T. ) ;
#10746 = ORIENTED_EDGE ( 'NONE', *, *, #3786, .T. ) ;
#10748 = ORIENTED_EDGE ( 'NONE', *, *, #20890, .F. ) ;
#10749 = ORIENTED_EDGE ( 'NONE', *, *, #3887, .F. ) ;
#10750 = ORIENTED_EDGE ( 'NONE', *, *, #14821, .T. ) ;
#10751 = PLANE ( 'NONE',  #7311 ) ;
#10752 = VECTOR ( 'NONE', #2327, 1000.000000000000000 ) ;
#10753 = CARTESIAN_POINT ( 'NONE',  ( -8.223343937052071340, -13.45452499186315443, 7.291631794411082446 ) ) ;
#10754 = CYLINDRICAL_SURFACE ( 'NONE', #4965, 0.4999999999999982236 ) ;
#10755 = AXIS2_PLACEMENT_3D ( 'NONE', #9816, #881, #2517 ) ;
#10756 = CARTESIAN_POINT ( 'NONE',  ( 3.999999999999989786, -2.309401076758549998, -5.242734410091827613 ) ) ;
#10757 = DIRECTION ( 'NONE',  ( 2.013525853228507892E-32, 6.902532920683810383E-31, -1.000000000000000000 ) ) ;
#10758 = CARTESIAN_POINT ( 'NONE',  ( -4.140404888673358208, -2.228338276487483505, -3.686887068327060035 ) ) ;
#10759 =( NAMED_UNIT ( * ) PLANE_ANGLE_UNIT ( ) SI_UNIT ( $, .RADIAN. ) );
#10760 = CARTESIAN_POINT ( 'NONE',  ( 5.599999999999994316, -2.020725942163695166, -3.500000000000007550 ) ) ;
#10761 = LINE ( 'NONE', #17950, #11177 ) ;
#10762 = DIRECTION ( 'NONE',  ( -4.190823558986625216E-31, 1.000000000000000000, -4.190823558986625216E-31 ) ) ;
#10763 = B_SPLINE_CURVE_WITH_KNOTS ( 'NONE', 3,
 ( #20332, #4192, #2444, #14677, #9624, #16774 ),
 .UNSPECIFIED., .F., .F.,
 ( 4, 2, 4 ),
 ( 0.004120275011746843581, 0.005288420935197119671, 0.006456566858647396628 ),
 .UNSPECIFIED. ) ;
#10764 = DIRECTION ( 'NONE',  ( 1.000000000000000000, 0.000000000000000000, 0.000000000000000000 ) ) ;
#10765 =( BOUNDED_SURFACE ( )  B_SPLINE_SURFACE ( 3, 2, ( 
 ( #13801, #1343, #8508 ),
 ( #6742, #995, #13914 ),
 ( #4966, #15783, #2744 ),
 ( #21229, #5095, #18862 ),
 ( #9931, #20874, #8161 ),
 ( #15329, #13574, #20759 ) ),
 .UNSPECIFIED., .F., .F., .F. ) 
 B_SPLINE_SURFACE_WITH_KNOTS ( ( 4, 2, 4 ),
 ( 3, 3 ),
 ( 0.01651732063679901830, 0.01857756227444014308, 0.02063780391208126438 ),
 ( 0.000000000000000000, 1.000000000000000000 ),
 .UNSPECIFIED. ) 
 GEOMETRIC_REPRESENTATION_ITEM ( )  RATIONAL_B_SPLINE_SURFACE ( (
 ( 1.000000000000000000, 0.8047781231227495446, 1.000000000000000000),
 ( 1.000000000000000000, 0.8123782108665584811, 1.000000000000000000),
 ( 1.000000000000000000, 0.8190665102132670405, 1.000000000000000000),
 ( 1.000000000000000000, 0.8192358432844795146, 1.000000000000000000),
 ( 1.000000000000000000, 0.8126132624434716512, 1.000000000000000000),
 ( 1.000000000000000000, 0.8047712436238877443, 1.000000000000000000) ) ) 
 REPRESENTATION_ITEM ( '' )  SURFACE ( )  );
#10766 = EDGE_LOOP ( 'NONE', ( #23071, #13590, #21419, #14855 ) ) ;
#10767 = TOROIDAL_SURFACE ( 'NONE', #11511, 4.500000000000000888, 0.5000000000000000000 ) ;
#10768 = CARTESIAN_POINT ( 'NONE',  ( 88.75737332930594903, -6.527605602963476805, 6.500000000000151879 ) ) ;
#10769 = DIRECTION ( 'NONE',  ( 1.000000000000000000, 2.220446049250313081E-16, -3.656342123407315983E-48 ) ) ;
#10771 = ORIENTED_EDGE ( 'NONE', *, *, #22174, .T. ) ;
#10770 = VERTEX_POINT ( 'NONE', #20574 ) ;
#10772 = VECTOR ( 'NONE', #14278, 1000.000000000000000 ) ;
#10773 = ORIENTED_EDGE ( 'NONE', *, *, #23059, .T. ) ;
#10774 = ORIENTED_EDGE ( 'NONE', *, *, #20074, .F. ) ;
#10775 = AXIS2_PLACEMENT_3D ( 'NONE', #8863, #8512, #49 ) ;
#10776 = ORIENTED_EDGE ( 'NONE', *, *, #7124, .T. ) ;
#10777 = ORIENTED_EDGE ( 'NONE', *, *, #13484, .T. ) ;
#10778 = EDGE_CURVE ( 'NONE', #8087, #17188, #18190, .T. ) ;
#10779 = DIRECTION ( 'NONE',  ( -1.000000000000000000, 4.190823558986610327E-31, -1.733449886265890494E-32 ) ) ;
#10780 = CARTESIAN_POINT ( 'NONE',  ( -2.500000000000000000, 2.761527815601792292E-14, -1.965053746193064019E-17 ) ) ;
#10781 = DIRECTION ( 'NONE',  ( 1.134196829589822059E-15, 6.741645191078038822E-32, -1.000000000000000000 ) ) ;
#10782 = CARTESIAN_POINT ( 'NONE',  ( 4.175572532730925879, -2.061029303918069377, -3.569807470274383832 ) ) ;
#10783 = CARTESIAN_POINT ( 'NONE',  ( 0.000000000000000000, -1.750000000000001554, 0.000000000000000000 ) ) ;
#10784 = PLANE ( 'NONE',  #7506 ) ;
#10785 = DIRECTION ( 'NONE',  ( 0.000000000000000000, -1.000000000000000000, 0.000000000000000000 ) ) ;
#10786 = CARTESIAN_POINT ( 'NONE',  ( 66.26395429947839943, 0.000000000000000000, 6.000000000000178524 ) ) ;
#10787 = TOROIDAL_SURFACE ( 'NONE', #20931, 5.200000000000001066, 0.4999999999999978351 ) ;
#10788 = DIRECTION ( 'NONE',  ( -9.121204216617949000E-31, -1.000000000000000000, 6.982962677686261977E-15 ) ) ;
#10789 = CARTESIAN_POINT ( 'NONE',  ( 37.86602540378461157, 11.00000000000000533, -10.86602540378452275 ) ) ;
#10790 = MECHANICAL_DESIGN_GEOMETRIC_PRESENTATION_REPRESENTATION (  '', ( #5908 ), #16400 ) ;
#10791 = DIRECTION ( 'NONE',  ( 0.7071067811865534569, 0.7071067811865416886, 1.565905175853764455E-16 ) ) ;
#10792 = EDGE_CURVE ( 'NONE', #7125, #17822, #20434, .T. ) ;
#10793 = FACE_OUTER_BOUND ( 'NONE', #22763, .T. ) ;
#10794 = VECTOR ( 'NONE', #11973, 1000.000000000000000 ) ;
#10795 = DIRECTION ( 'NONE',  ( 6.656013887802287108E-31, 1.000000000000000000, -3.469446951953609061E-15 ) ) ;
#10796 = ORIENTED_EDGE ( 'NONE', *, *, #2964, .F. ) ;
#10797 = VECTOR ( 'NONE', #8982, 1000.000000000000000 ) ;
#10798 = EDGE_CURVE ( 'NONE', #2694, #17301, #909, .T. ) ;
#10799 = ORIENTED_EDGE ( 'NONE', *, *, #67, .F. ) ;
#10800 = AXIS2_PLACEMENT_3D ( 'NONE', #17142, #6582, #15734 ) ;
#10801 = CIRCLE ( 'NONE', #282, 0.2500000000000002220 ) ;
#10802 = EDGE_CURVE ( 'NONE', #17658, #14732, #13296, .T. ) ;
#10803 = DIRECTION ( 'NONE',  ( 1.000000000000000000, -4.615739097524200579E-16, -1.134196829589820086E-15 ) ) ;
#10804 = EDGE_LOOP ( 'NONE', ( #5314, #18997, #7545, #3693, #1721, #7974 ) ) ;
#10805 = VECTOR ( 'NONE', #7866, 1000.000000000000000 ) ;
#10806 = CARTESIAN_POINT ( 'NONE',  ( 0.5276280594149747039, -4.314175951381801433, -3.320322319201818750 ) ) ;
#10807 = DIRECTION ( 'NONE',  ( 8.438582421954109416E-32, 0.000000000000000000, 1.000000000000000000 ) ) ;
#10808 = CARTESIAN_POINT ( 'NONE',  ( 3.880206590543044953, -2.665671387532588366, -2.382921720511024244 ) ) ;
#10809 = AXIS2_PLACEMENT_3D ( 'NONE', #12613, #1690, #16135 ) ;
#10810 = EDGE_CURVE ( 'NONE', #8517, #15515, #2921, .T. ) ;
#10811 = DIRECTION ( 'NONE',  ( -1.000000000000000000, 0.000000000000000000, -3.717264591378832268E-16 ) ) ;
#10812 = CARTESIAN_POINT ( 'NONE',  ( 0.4414465083558130054, 0.6000000000000127454, -4.146294842461959895 ) ) ;
#10813 = EDGE_CURVE ( 'NONE', #405, #7652, #7598, .T. ) ;
#10814 = DIRECTION ( 'NONE',  ( -0.6819983600624998088, -0.7313537016191693496, 0.000000000000000000 ) ) ;
#10815 = AXIS2_PLACEMENT_3D ( 'NONE', #17556, #3228, #1564 ) ;
#10816 = CARTESIAN_POINT ( 'NONE',  ( -3.499999999708153453, 42.99999999900385461, -18.50000000000000355 ) ) ;
#10817 = LINE ( 'NONE', #10351, #14826 ) ;
#10818 = CARTESIAN_POINT ( 'NONE',  ( 8.518530740349840258, -2.043531002858649082, 6.984205661427222545 ) ) ;
#10819 = CARTESIAN_POINT ( 'NONE',  ( 4.082498951862917558, 2.020725942163638766, -3.499999999999997780 ) ) ;
#10820 = DIRECTION ( 'NONE',  ( -0.000000000000000000, 0.000000000000000000, -1.000000000000000000 ) ) ;
#10821 = CARTESIAN_POINT ( 'NONE',  ( -3.880358743661353138, 1.739972214219164925, 2.779021504384385999 ) ) ;
#10822 = AXIS2_PLACEMENT_3D ( 'NONE', #6867, #1348, #3573 ) ;
#10823 = CARTESIAN_POINT ( 'NONE',  ( 0.2175679805410084544, -1.691499766303321106, 3.499999999999993783 ) ) ;
#10824 = CIRCLE ( 'NONE', #322, 2.500000000000001332 ) ;
#10825 = EDGE_CURVE ( 'NONE', #9571, #17483, #17369, .T. ) ;
#10826 = ORIENTED_EDGE ( 'NONE', *, *, #8855, .F. ) ;
#10827 = EDGE_CURVE ( 'NONE', #19001, #19925, #5501, .T. ) ;
#10828 = CIRCLE ( 'NONE', #4830, 2.500000000000002220 ) ;
#10829 = ADVANCED_FACE ( 'NONE', ( #10322 ), #1728, .T. ) ;
#10830 = APPLICATION_PROTOCOL_DEFINITION ( 'draft international standard', 'automotive_design', 1998, #18364 ) ;
#10832 = EDGE_LOOP ( 'NONE', ( #15311, #10304, #15338, #22736, #20620, #4727, #4953, #9364 ) ) ;
#10831 = VERTEX_POINT ( 'NONE', #23160 ) ;
#10834 = ORIENTED_EDGE ( 'NONE', *, *, #7586, .F. ) ;
#10833 = ORIENTED_EDGE ( 'NONE', *, *, #11811, .F. ) ;
#10835 = ADVANCED_FACE ( 'NONE', ( #12660 ), #1961, .T. ) ;
#10836 = DIRECTION ( 'NONE',  ( 1.000000000000000000, -1.276756478318923119E-15, 1.403805528459192781E-15 ) ) ;
#10837 = CARTESIAN_POINT ( 'NONE',  ( 37.86602540378462578, -1.973247953923618070E-14, -2.133974596215460817 ) ) ;
#10838 = CARTESIAN_POINT ( 'NONE',  ( 8.216162181246577489, -12.44282262938666328, 7.299847320220921532 ) ) ;
#10839 = EDGE_CURVE ( 'NONE', #19780, #17901, #19623, .T. ) ;
#10840 = CARTESIAN_POINT ( 'NONE',  ( 1.387778780781445676E-16, -7.172549406584475716E-16, -2.499999999999993783 ) ) ;
#10841 = DIRECTION ( 'NONE',  ( -3.254448077146059901E-32, -1.000000000000000000, -6.409494854920712161E-31 ) ) ;
#10842 = CARTESIAN_POINT ( 'NONE',  ( 3.938275312863521282, -0.7499999999999389377, -2.974550175612221459 ) ) ;
#10843 = CARTESIAN_POINT ( 'NONE',  ( 5.560781378645629047, -7.086303797513785838E-15, -4.000000000000000000 ) ) ;
#10844 = AXIS2_PLACEMENT_3D ( 'NONE', #4083, #7732, #11259 ) ;
#10845 = AXIS2_PLACEMENT_3D ( 'NONE', #4299, #13144, #20319 ) ;
#10846 = FACE_OUTER_BOUND ( 'NONE', #10274, .T. ) ;
#10847 = AXIS2_PLACEMENT_3D ( 'NONE', #15559, #9697, #13344 ) ;
#10848 = CARTESIAN_POINT ( 'NONE',  ( 5.484827557301438894, 1.749999999999998002, -2.775557561562891351E-14 ) ) ;
#10849 = DIRECTION ( 'NONE',  ( 1.000000000000000000, 3.254448077276381206E-32, 1.066788928082016908E-26 ) ) ;
#10850 = CARTESIAN_POINT ( 'NONE',  ( 42.00000000000014921, 8.000000000000003553, 2.500000000000030198 ) ) ;
#10851 = B_SPLINE_CURVE_WITH_KNOTS ( 'NONE', 3,
 ( #2373, #16712, #22254, #7086 ),
 .UNSPECIFIED., .F., .F.,
 ( 4, 4 ),
 ( 0.000000000000000000, 0.002080789711329261542 ),
 .UNSPECIFIED. ) ;
#10852 = DIRECTION ( 'NONE',  ( 1.454462294001240516E-30, 1.000000000000000000, 0.000000000000000000 ) ) ;
#10853 = DIRECTION ( 'NONE',  ( -0.7071067811865541231, 0.7071067811865411334, 1.565905175853764948E-16 ) ) ;
#10854 = CARTESIAN_POINT ( 'NONE',  ( 7.951003271401690498, -0.1617022081438048986, 7.659883344695789020 ) ) ;
#10855 = ORIENTED_EDGE ( 'NONE', *, *, #19686, .F. ) ;
#10857 = VERTEX_POINT ( 'NONE', #15730 ) ;
#10856 = ORIENTED_EDGE ( 'NONE', *, *, #20173, .T. ) ;
#10858 = VERTEX_POINT ( 'NONE', #5028 ) ;
#10859 = AXIS2_PLACEMENT_3D ( 'NONE', #14074, #21263, #12533 ) ;
#10861 = ORIENTED_EDGE ( 'NONE', *, *, #18215, .F. ) ;
#10860 = ORIENTED_EDGE ( 'NONE', *, *, #12556, .F. ) ;
#10862 = ORIENTED_EDGE ( 'NONE', *, *, #21508, .F. ) ;
#10863 = EDGE_CURVE ( 'NONE', #14796, #15246, #1228, .T. ) ;
#10864 = ORIENTED_EDGE ( 'NONE', *, *, #1875, .T. ) ;
#10865 = ORIENTED_EDGE ( 'NONE', *, *, #6503, .F. ) ;
#10866 = CARTESIAN_POINT ( 'NONE',  ( 4.000000000000004441, 0.7862748000878158061, -0.03447227762756879116 ) ) ;
#10867 = VECTOR ( 'NONE', #3416, 1000.000000000000114 ) ;
#10868 = PLANE ( 'NONE',  #20676 ) ;
#10869 = EDGE_CURVE ( 'NONE', #5312, #20860, #1617, .T. ) ;
#10870 = CARTESIAN_POINT ( 'NONE',  ( 12.84999999999997300, -13.50000000000007105, 5.551115123125782702E-14 ) ) ;
#10871 = CARTESIAN_POINT ( 'NONE',  ( 4.082498951862921999, -2.020725942163709377, -3.499999999999999556 ) ) ;
#10872 = FACE_OUTER_BOUND ( 'NONE', #22991, .T. ) ;
#10873 = DIRECTION ( 'NONE',  ( -1.000000000000000000, 0.000000000000000000, 0.000000000000000000 ) ) ;
#10874 =( LENGTH_UNIT ( ) NAMED_UNIT ( * ) SI_UNIT ( .MILLI., .METRE. ) );
#10875 = DIRECTION ( 'NONE',  ( 0.7313537016191730133, -0.6819983600624959230, 5.924440990721418971E-17 ) ) ;
#10876 = DIRECTION ( 'NONE',  ( 5.551115123125796261E-17, -2.869019762633797485E-16, -1.000000000000000000 ) ) ;
#10877 = EDGE_CURVE ( 'NONE', #1743, #9669, #17614, .T. ) ;
#10878 = CARTESIAN_POINT ( 'NONE',  ( 37.69160037009668685, 10.97664592903650060, -2.482824663591210346 ) ) ;
#10879 = ORIENTED_EDGE ( 'NONE', *, *, #979, .F. ) ;
#10880 = FACE_OUTER_BOUND ( 'NONE', #23089, .T. ) ;
#10881 = VECTOR ( 'NONE', #17580, 1000.000000000000227 ) ;
#10883 = ORIENTED_EDGE ( 'NONE', *, *, #22036, .F. ) ;
#10882 = ORIENTED_EDGE ( 'NONE', *, *, #14353, .T. ) ;
#10884 = COLOUR_RGB ( '', 0.40784314, 0.44705882, 0.49803922) ;
#10885 = ORIENTED_EDGE ( 'NONE', *, *, #9307, .T. ) ;
#10886 = VERTEX_POINT ( 'NONE', #8676 ) ;
#10887 = FACE_OUTER_BOUND ( 'NONE', #20113, .T. ) ;
#10888 = DIRECTION ( 'NONE',  ( -2.013525853228507892E-32, -6.902532920683810383E-31, 1.000000000000000000 ) ) ;
#10889 = DIRECTION ( 'NONE',  ( 4.336808689942045346E-15, -1.000000000000000000, -7.518830502887770522E-31 ) ) ;
#10890 = CARTESIAN_POINT ( 'NONE',  ( 4.158413352280815545, -2.044871626972824430, -3.541821552872962187 ) ) ;
#10891 = DIRECTION ( 'NONE',  ( 0.000000000000000000, 0.000000000000000000, 1.000000000000000000 ) ) ;
#10892 = DIRECTION ( 'NONE',  ( -1.000000000000000000, -1.479114197289397135E-31, -5.916456789157588541E-31 ) ) ;
#10893 = AXIS2_PLACEMENT_3D ( 'NONE', #12724, #14834, #13072 ) ;
#10894 = DIRECTION ( 'NONE',  ( 1.000000000000000000, 1.479114197289388027E-30, -2.013525853228518840E-32 ) ) ;
#10895 = CARTESIAN_POINT ( 'NONE',  ( -56.87767137932630845, 2.700000000000098321, 8.833333333333415638 ) ) ;
#10896 = CARTESIAN_POINT ( 'NONE',  ( -6.000000000000047073, -5.300000000000006040, 8.000000000000090594 ) ) ;
#10897 = DIRECTION ( 'NONE',  ( 0.000000000000000000, 0.000000000000000000, -1.000000000000000000 ) ) ;
#10898 = CARTESIAN_POINT ( 'NONE',  ( -8.697224362268011433, -14.00000000000004441, 6.250000000000033751 ) ) ;
#10899 = B_SPLINE_CURVE_WITH_KNOTS ( 'NONE', 3,
 ( #13602, #9959, #12045, #2655, #6313 ),
 .UNSPECIFIED., .F., .F.,
 ( 4, 1, 4 ),
 ( 0.000000000000000000, 0.002309401076758509259, 0.004618802153517017652 ),
 .UNSPECIFIED. ) ;
#10900 = DIRECTION ( 'NONE',  ( 3.885780586188016830E-16, 4.437342591868156373E-31, -1.000000000000000000 ) ) ;
#10901 = CARTESIAN_POINT ( 'NONE',  ( 37.35148779274771158, 0.3618892054749687226, -10.35148779274879693 ) ) ;
#10902 = EDGE_CURVE ( 'NONE', #7692, #8787, #13238, .T. ) ;
#10903 = CARTESIAN_POINT ( 'NONE',  ( -7.499999999999992895, -5.999999999999987566, 6.249999999999992006 ) ) ;
#10904 = CARTESIAN_POINT ( 'NONE',  ( -50.65685424949275983, 7.200000000000018829, -8.000000000000007105 ) ) ;
#10905 = VERTEX_POINT ( 'NONE', #19739 ) ;
#10906 = EDGE_LOOP ( 'NONE', ( #18220, #23026, #15132, #1238 ) ) ;
#10907 = CARTESIAN_POINT ( 'NONE',  ( 61.83096495907203405, -4.753799060524588782, -5.999999999999956479 ) ) ;
#10908 = FACE_OUTER_BOUND ( 'NONE', #21183, .T. ) ;
#10909 = EDGE_LOOP ( 'NONE', ( #22913, #2412, #8269 ) ) ;
#10910 = CARTESIAN_POINT ( 'NONE',  ( 37.18301270189235908, 10.90849364905388263, -10.52451905283837874 ) ) ;
#10911 = CARTESIAN_POINT ( 'NONE',  ( 30.00000000029184832, -9.961476088449217059E-10, -45.00000000000000000 ) ) ;
#10912 = LINE ( 'NONE', #7298, #21989 ) ;
#10913 = VERTEX_POINT ( 'NONE', #8912 ) ;
#10914 = CARTESIAN_POINT ( 'NONE',  ( 3.973110223765528914, -0.6902454861566355016, 3.565797985667388037 ) ) ;
#10915 = CARTESIAN_POINT ( 'NONE',  ( 0.5741843527964847205, 0.6000000000000127454, -4.263785792382347672 ) ) ;
#10916 = CARTESIAN_POINT ( 'NONE',  ( 0.000000000000000000, 0.000000000000000000, 3.499999999999999556 ) ) ;
#10917 = CYLINDRICAL_SURFACE ( 'NONE', #18188, 0.4999999999999978351 ) ;
#10918 = CARTESIAN_POINT ( 'NONE',  ( 8.233775472210654200, -13.45629277298760584, 7.279685395985904250 ) ) ;
#10919 = CARTESIAN_POINT ( 'NONE',  ( 8.954763739086866181, -1.999999999999987343, 6.678571428571431490 ) ) ;
#10920 = CIRCLE ( 'NONE', #15066, 0.4999999999999995559 ) ;
#10921 = CIRCLE ( 'NONE', #12814, 10.00000000000006395 ) ;
#10922 = CARTESIAN_POINT ( 'NONE',  ( -6.000000000000019540, -4.800000000000006040, 7.500000000000062172 ) ) ;
#10923 = CARTESIAN_POINT ( 'NONE',  ( 3.880206590543190170, -3.396506438958537988, 1.117078279489006620 ) ) ;
#10924 = CARTESIAN_POINT ( 'NONE',  ( -3.191783008269886146, 1.561572887838377666, 3.971669662941508694 ) ) ;
#10925 = EDGE_CURVE ( 'NONE', #10008, #178, #17740, .T. ) ;
#10926 = CARTESIAN_POINT ( 'NONE',  ( 3.000000000291852764, 42.99999999900385461, -25.50000000000000355 ) ) ;
#10927 = ORIENTED_EDGE ( 'NONE', *, *, #13816, .T. ) ;
#10928 = EDGE_CURVE ( 'NONE', #19419, #7917, #4205, .T. ) ;
#10929 = APPLICATION_PROTOCOL_DEFINITION ( 'draft international standard', 'automotive_design', 1998, #21574 ) ;
#10930 = EDGE_CURVE ( 'NONE', #9421, #13451, #2717, .T. ) ;
#10932 = ORIENTED_EDGE ( 'NONE', *, *, #8072, .F. ) ;
#10931 = ORIENTED_EDGE ( 'NONE', *, *, #2006, .F. ) ;
#10933 = EDGE_CURVE ( 'NONE', #3970, #371, #23024, .T. ) ;
#10934 = EDGE_LOOP ( 'NONE', ( #15216, #3184, #2721, #13591 ) ) ;
#10936 = ORIENTED_EDGE ( 'NONE', *, *, #20005, .T. ) ;
#10935 = EDGE_LOOP ( 'NONE', ( #7225, #14046, #5916, #14136 ) ) ;
#10937 = CIRCLE ( 'NONE', #15458, 4.000000000000000000 ) ;
#10938 = AXIS2_PLACEMENT_3D ( 'NONE', #15295, #4349, #22486 ) ;
#10939 = DIRECTION ( 'NONE',  ( -3.032184104443272185E-30, -1.000000000000000000, 7.395570986447005381E-32 ) ) ;
#10940 = CARTESIAN_POINT ( 'NONE',  ( 37.04362427881587649, 0.2122202663360489572, -2.545175158706924012 ) ) ;
#10941 = CARTESIAN_POINT ( 'NONE',  ( 8.498922697886598598, -12.49080420435820926, 6.997949321565184455 ) ) ;
#10942 = CARTESIAN_POINT ( 'NONE',  ( -7.162073728446670451, -11.63471678239051954, 7.945145523438286617 ) ) ;
#10943 = DIRECTION ( 'NONE',  ( 1.000000000000000000, 2.168404344970992105E-16, 0.000000000000000000 ) ) ;
#10944 = LINE ( 'NONE', #17666, #7628 ) ;
#10946 = EDGE_CURVE ( 'NONE', #15916, #21787, #9868, .T. ) ;
#10945 = DIRECTION ( 'NONE',  ( -1.000000000000000000, -1.479114197289388027E-30, 2.013525853228518840E-32 ) ) ;
#10947 = EDGE_CURVE ( 'NONE', #15196, #6879, #3469, .T. ) ;
#10948 = DIRECTION ( 'NONE',  ( -1.276756478318923119E-15, -1.000000000000000000, 2.778352770573917478E-17 ) ) ;
#10949 = DIRECTION ( 'NONE',  ( 2.013525853228507892E-32, 6.902532920683810383E-31, -1.000000000000000000 ) ) ;
#10950 = CARTESIAN_POINT ( 'NONE',  ( 1.499999999999997780, -2.098699259529624113E-31, 3.113037248396080425 ) ) ;
#10951 = DIRECTION ( 'NONE',  ( 1.000000000000000000, 4.440892098500626162E-16, -5.551115123125782702E-16 ) ) ;
#10952 = CARTESIAN_POINT ( 'NONE',  ( 66.26395429947831417, -4.500000000000003553, 6.000000000000192735 ) ) ;
#10953 = FACE_BOUND ( 'NONE', #16951, .T. ) ;
#10954 = AXIS2_PLACEMENT_3D ( 'NONE', #7605, #11249, #672 ) ;
#10955 = AXIS2_PLACEMENT_3D ( 'NONE', #8675, #19497, #11962 ) ;
#10956 = CARTESIAN_POINT ( 'NONE',  ( -6.219322015043732499, 35.99999999900384040, -18.99225239120474740 ) ) ;
#10957 = EDGE_CURVE ( 'NONE', #16094, #13530, #1583, .T. ) ;
#10958 = DIRECTION ( 'NONE',  ( -1.000000000000000000, 1.626303258728244079E-16, 0.000000000000000000 ) ) ;
#10959 = ORIENTED_EDGE ( 'NONE', *, *, #2522, .T. ) ;
#10960 = EDGE_CURVE ( 'NONE', #22262, #12387, #10555, .T. ) ;
#10962 = VERTEX_POINT ( 'NONE', #14212 ) ;
#10961 = ORIENTED_EDGE ( 'NONE', *, *, #16981, .F. ) ;
#10963 = UNCERTAINTY_MEASURE_WITH_UNIT (LENGTH_MEASURE( 1.000000000000000082E-05 ), #10874, 'distance_accuracy_value', 'NONE');
#10964 = EDGE_CURVE ( 'NONE', #15768, #9602, #15106, .T. ) ;
#10965 = ORIENTED_EDGE ( 'NONE', *, *, #4311, .F. ) ;
#10967 = ORIENTED_EDGE ( 'NONE', *, *, #22043, .F. ) ;
#10966 = VERTEX_POINT ( 'NONE', #3499 ) ;
#10968 = EDGE_CURVE ( 'NONE', #4546, #9468, #22631, .T. ) ;
#10969 = ORIENTED_EDGE ( 'NONE', *, *, #6232, .F. ) ;
#10970 = ORIENTED_EDGE ( 'NONE', *, *, #2180, .F. ) ;
#10971 = CARTESIAN_POINT ( 'NONE',  ( 7.000000000000020428, -13.02884243125069652, 9.522727272727321335 ) ) ;
#10972 = EDGE_LOOP ( 'NONE', ( #16545, #22232, #16000, #20738, #6359, #21497 ) ) ;
#10973 = VERTEX_POINT ( 'NONE', #22190 ) ;
#10974 = CARTESIAN_POINT ( 'NONE',  ( -12.84999999999999964, -0.5000000000000004441, -5.749999999999963585 ) ) ;
#10975 = AXIS2_PLACEMENT_3D ( 'NONE', #2631, #13216, #4041 ) ;
#10976 = DIRECTION ( 'NONE',  ( -1.000000000000000000, 0.000000000000000000, 0.000000000000000000 ) ) ;
#10977 = VECTOR ( 'NONE', #1502, 1000.000000000000114 ) ;
#10978 = DIRECTION ( 'NONE',  ( -1.000000000000000000, -1.424116703980846297E-16, 1.095779650622964657E-32 ) ) ;
#10979 = CIRCLE ( 'NONE', #13615, 0.5000000000000022204 ) ;
#10980 = DIRECTION ( 'NONE',  ( 0.7071067811865475727, -0.7071067811865475727, 0.000000000000000000 ) ) ;
#10981 = VECTOR ( 'NONE', #12304, 1000.000000000000000 ) ;
#10982 = ADVANCED_FACE ( 'NONE', ( #20312 ), #13019, .F. ) ;
#10983 = CARTESIAN_POINT ( 'NONE',  ( -90.55603112840523750, -0.5000000000000628386, -7.432974388601742533 ) ) ;
#10984 = CARTESIAN_POINT ( 'NONE',  ( 108.2426266706970637, -13.52760560296348302, 6.500000000000019540 ) ) ;
#10985 = DIRECTION ( 'NONE',  ( 1.714307746994311415E-19, -0.7904150521752424385, -0.6125716654358157598 ) ) ;
#10986 = FILL_AREA_STYLE ('',( #7358 ) ) ;
#10987 = DIRECTION ( 'NONE',  ( -1.000000000000000000, -2.699383410053119644E-30, -3.330669073875432643E-16 ) ) ;
#10988 = VECTOR ( 'NONE', #501, 1000.000000000000000 ) ;
#10989 = DIRECTION ( 'NONE',  ( -1.000000000000000000, -1.479114197289397135E-31, -5.916456789157588541E-31 ) ) ;
#10990 = EDGE_CURVE ( 'NONE', #22002, #2089, #11585, .T. ) ;
#10991 = CARTESIAN_POINT ( 'NONE',  ( -45.37157287525420202, 6.828427124746163202, 7.500000000000089706 ) ) ;
#10992 = ORIENTED_EDGE ( 'NONE', *, *, #4025, .F. ) ;
#10993 = PRODUCT_DEFINITION_CONTEXT ( 'detailed design', #22003, 'design' ) ;
#10994 = DIRECTION ( 'NONE',  ( -9.693522803355793065E-26, 5.963788443470849249E-28, 1.000000000000000000 ) ) ;
#10995 = AXIS2_PLACEMENT_3D ( 'NONE', #11068, #11297, #18478 ) ;
#10997 = ORIENTED_EDGE ( 'NONE', *, *, #21959, .F. ) ;
#10996 = ORIENTED_EDGE ( 'NONE', *, *, #926, .F. ) ;
#10998 = AXIS2_PLACEMENT_3D ( 'NONE', #21368, #17462, #22768 ) ;
#10999 = VECTOR ( 'NONE', #17830, 1000.000000000000000 ) ;
#11000 = AXIS2_PLACEMENT_3D ( 'NONE', #1436, #20865, #11899 ) ;
#11001 = VERTEX_POINT ( 'NONE', #20084 ) ;
#11002 = VERTEX_POINT ( 'NONE', #21844 ) ;
#11003 = VERTEX_POINT ( 'NONE', #9484 ) ;
#11004 = ORIENTED_EDGE ( 'NONE', *, *, #18844, .T. ) ;
#11005 = DIRECTION ( 'NONE',  ( -3.330669073875432643E-16, -4.437342591868153746E-31, 1.000000000000000000 ) ) ;
#11006 = CARTESIAN_POINT ( 'NONE',  ( 8.954763739086866181, -12.50000000000002132, 6.678571428571491886 ) ) ;
#11007 = CARTESIAN_POINT ( 'NONE',  ( 4.104070371397483541, -2.023683613428369110, -3.505122836902508698 ) ) ;
#11008 = AXIS2_PLACEMENT_3D ( 'NONE', #3511, #3284, #12436 ) ;
#11009 = CARTESIAN_POINT ( 'NONE',  ( -89.70000000000057128, -9.020562075079396891E-14, -2.000000000000001776 ) ) ;
#11010 = VECTOR ( 'NONE', #21826, 1000.000000000000000 ) ;
#11011 = CYLINDRICAL_SURFACE ( 'NONE', #11981, 0.5000000000000037748 ) ;
#11012 = DIRECTION ( 'NONE',  ( -2.775557561562890735E-17, 3.352716401118095686E-16, -1.000000000000000000 ) ) ;
#11013 = VECTOR ( 'NONE', #15861, 1000.000000000000114 ) ;
#11014 = AXIS2_PLACEMENT_3D ( 'NONE', #17669, #10609, #12962 ) ;
#11015 = DIRECTION ( 'NONE',  ( 0.000000000000000000, 0.000000000000000000, 1.000000000000000000 ) ) ;
#11017 = ADVANCED_FACE ( 'NONE', ( #319 ), #12779, .F. ) ;
#11016 = AXIS2_PLACEMENT_3D ( 'NONE', #5087, #8385, #1216 ) ;
#11018 = CARTESIAN_POINT ( 'NONE',  ( -7.499999999999994671, -13.02884243125068586, 9.522727272727351533 ) ) ;
#11019 = DIRECTION ( 'NONE',  ( -1.392757777031969319E-14, -1.000000000000000000, 5.941108692445745160E-30 ) ) ;
#11020 = CARTESIAN_POINT ( 'NONE',  ( 1.387778780781445676E-14, 4.857225732735059864E-14, -1.500000000000001332 ) ) ;
#11021 = LINE ( 'NONE', #14668, #3287 ) ;
#11022 = EDGE_CURVE ( 'NONE', #12892, #16286, #11719, .T. ) ;
#11023 = LINE ( 'NONE', #11359, #19028 ) ;
#11024 = DIRECTION ( 'NONE',  ( -5.551115123561405253E-17, -1.000000000000000000, -2.256980353643891447E-27 ) ) ;
#11025 = CARTESIAN_POINT ( 'NONE',  ( -45.01801948466080461, -6.474873734152907900, -8.000000000000035527 ) ) ;
#11026 = ORIENTED_EDGE ( 'NONE', *, *, #5139, .T. ) ;
#11027 = EDGE_CURVE ( 'NONE', #21952, #4281, #18424, .T. ) ;
#11028 = AXIS2_PLACEMENT_3D ( 'NONE', #795, #20440, #6204 ) ;
#11029 = ORIENTED_EDGE ( 'NONE', *, *, #9941, .F. ) ;
#11030 = AXIS2_PLACEMENT_3D ( 'NONE', #2809, #4442, #17023 ) ;
#11031 = VECTOR ( 'NONE', #4170, 1000.000000000000114 ) ;
#11032 = CARTESIAN_POINT ( 'NONE',  ( -42.54314575050785407, -7.500000000000020428, 8.000000000000007105 ) ) ;
#11033 = CARTESIAN_POINT ( 'NONE',  ( -4.499999999708154341, 36.49999999900384751, -19.50000000000000355 ) ) ;
#11034 = ORIENTED_EDGE ( 'NONE', *, *, #974, .T. ) ;
#11035 = DIRECTION ( 'NONE',  ( 1.000000000000000000, 0.000000000000000000, 0.000000000000000000 ) ) ;
#11036 = LINE ( 'NONE', #12804, #4738 ) ;
#11037 = CARTESIAN_POINT ( 'NONE',  ( 7.761744141695591459, -11.93564195219169299, 6.973942750959585268 ) ) ;
#11038 = PLANE ( 'NONE',  #19603 ) ;
#11039 = DIRECTION ( 'NONE',  ( -0.000000000000000000, -0.000000000000000000, 1.000000000000000000 ) ) ;
#11040 = ORIENTED_EDGE ( 'NONE', *, *, #78, .F. ) ;
#11041 = CARTESIAN_POINT ( 'NONE',  ( -3.999999999708153453, 36.49999999900384751, -26.00000000000000000 ) ) ;
#11042 = CARTESIAN_POINT ( 'NONE',  ( -4.101948962586008385, -2.368261337751097706, -3.681124513963646372 ) ) ;
#11043 = PLANE ( 'NONE',  #15049 ) ;
#11044 = CARTESIAN_POINT ( 'NONE',  ( -6.999999999708156118, 6.999999999003851947, -26.00000000000000000 ) ) ;
#11045 = CARTESIAN_POINT ( 'NONE',  ( 7.525553787417719853, -12.92907334721305368, 8.786654903594133259 ) ) ;
#11046 = AXIS2_PLACEMENT_3D ( 'NONE', #22980, #6856, #7110 ) ;
#11047 = CARTESIAN_POINT ( 'NONE',  ( -4.000000000000096811, -0.3979232138631050297, -6.754240721405789642E-14 ) ) ;
#11048 = AXIS2_PLACEMENT_3D ( 'NONE', #16950, #1215, #18977 ) ;
#11049 = AXIS2_PLACEMENT_3D ( 'NONE', #5453, #3446, #3343 ) ;
#11050 = CARTESIAN_POINT ( 'NONE',  ( 4.158806965674309630, 4.075748668183996060, 0.05940377217582432784 ) ) ;
#11051 = LINE ( 'NONE', #14928, #5592 ) ;
#11052 = AXIS2_PLACEMENT_3D ( 'NONE', #14171, #14054, #19347 ) ;
#11053 = FILL_AREA_STYLE ('',( #20347 ) ) ;
#11054 = LINE ( 'NONE', #17772, #20594 ) ;
#11055 = PRODUCT_CONTEXT ( 'NONE', #12687, 'mechanical' ) ;
#11056 = ORIENTED_EDGE ( 'NONE', *, *, #11287, .F. ) ;
#11057 = EDGE_LOOP ( 'NONE', ( #3910, #15603, #8488, #6043 ) ) ;
#11058 = PRODUCT_DEFINITION ( 'UNKNOWN', '', #4485, #22059 ) ;
#11059 = AXIS2_PLACEMENT_3D ( 'NONE', #21796, #3897, #16475 ) ;
#11061 = EDGE_LOOP ( 'NONE', ( #6753, #17778, #22968, #18973 ) ) ;
#11060 = ORIENTED_EDGE ( 'NONE', *, *, #788, .F. ) ;
#11062 = AXIS2_PLACEMENT_3D ( 'NONE', #2621, #9797, #4732 ) ;
#11063 = PLANE ( 'NONE',  #6903 ) ;
#11064 = CARTESIAN_POINT ( 'NONE',  ( 37.36637401601597475, 0.3137297356303543339, -2.633625983984334340 ) ) ;
#11065 = ADVANCED_FACE ( 'NONE', ( #18313 ), #2303, .T. ) ;
#11066 = DIRECTION ( 'NONE',  ( 0.000000000000000000, 0.000000000000000000, 1.000000000000000000 ) ) ;
#11067 = DIRECTION ( 'NONE',  ( -0.000000000000000000, 1.000000000000000000, -0.000000000000000000 ) ) ;
#11068 = CARTESIAN_POINT ( 'NONE',  ( -0.5000000000000837108, -2.000000000000029310, 7.500000000000007105 ) ) ;
#11069 = CARTESIAN_POINT ( 'NONE',  ( 0.5724039806123020213, -0.5999999999999899858, -4.262472862582134425 ) ) ;
#11070 = EDGE_CURVE ( 'NONE', #4468, #3633, #8741, .T. ) ;
#11071 = FACE_BOUND ( 'NONE', #16486, .T. ) ;
#11072 = FACE_OUTER_BOUND ( 'NONE', #18906, .T. ) ;
#11073 = PLANE ( 'NONE',  #2364 ) ;
#11074 = DIRECTION ( 'NONE',  ( -1.000000000000000000, -1.479114197289387852E-30, 2.013525853228518840E-32 ) ) ;
#11075 = VECTOR ( 'NONE', #13635, 1000.000000000000000 ) ;
#11076 = CIRCLE ( 'NONE', #2827, 2.550000000000010481 ) ;
#11077 = CARTESIAN_POINT ( 'NONE',  ( 8.438463404362677167, -2.001835333048895826, 6.398712851742186736 ) ) ;
#11078 = LINE ( 'NONE', #14502, #15679 ) ;
#11079 = EDGE_CURVE ( 'NONE', #9470, #10566, #210, .T. ) ;
#11080 = CARTESIAN_POINT ( 'NONE',  ( 4.630153689607052314, 6.454774016259431095E-31, -5.371010071662833063 ) ) ;
#11081 = VERTEX_POINT ( 'NONE', #15005 ) ;
#11082 =( NAMED_UNIT ( * ) PLANE_ANGLE_UNIT ( ) SI_UNIT ( $, .RADIAN. ) );
#11084 = ORIENTED_EDGE ( 'NONE', *, *, #12794, .T. ) ;
#11083 = ORIENTED_EDGE ( 'NONE', *, *, #17731, .F. ) ;
#11085 = ORIENTED_EDGE ( 'NONE', *, *, #22498, .F. ) ;
#11086 = EDGE_CURVE ( 'NONE', #13358, #4671, #10979, .T. ) ;
#11088 = VERTEX_POINT ( 'NONE', #14892 ) ;
#11087 = VERTEX_POINT ( 'NONE', #19847 ) ;
#11089 = EDGE_LOOP ( 'NONE', ( #20942, #6784 ) ) ;
#11090 = CARTESIAN_POINT ( 'NONE',  ( -4.346882592290802982, -1.739972214219165370, 1.970978495615605341 ) ) ;
#11091 = ORIENTED_EDGE ( 'NONE', *, *, #17149, .F. ) ;
#11092 = EDGE_CURVE ( 'NONE', #10216, #16775, #6110, .T. ) ;
#11093 = VERTEX_POINT ( 'NONE', #9605 ) ;
#11094 = CARTESIAN_POINT ( 'NONE',  ( 0.2261952378970901179, 0.6000000000000133005, 3.877637771780682030 ) ) ;
#11095 =( GEOMETRIC_REPRESENTATION_CONTEXT ( 3 ) GLOBAL_UNCERTAINTY_ASSIGNED_CONTEXT ( ( #17299 ) ) GLOBAL_UNIT_ASSIGNED_CONTEXT ( ( #5172, #19639, #8349 ) ) REPRESENTATION_CONTEXT ( 'NONE', 'WORKASPACE' ) );
#11096 = CYLINDRICAL_SURFACE ( 'NONE', #1637, 2.499999999999993339 ) ;
#11097 = FACE_OUTER_BOUND ( 'NONE', #13650, .T. ) ;
#11098 = CARTESIAN_POINT ( 'NONE',  ( -6.999999999999992006, -3.018576030000268418, 8.916666666666687391 ) ) ;
#11099 = EDGE_CURVE ( 'NONE', #4944, #11150, #16757, .T. ) ;
#11100 = CARTESIAN_POINT ( 'NONE',  ( 0.000000000000000000, 0.000000000000000000, 0.000000000000000000 ) ) ;
#11101 = CARTESIAN_POINT ( 'NONE',  ( 7.000000000000006217, -1.390227771353540920, 9.250000000000021316 ) ) ;
#11102 = ADVANCED_FACE ( 'NONE', ( #18085 ), #853, .T. ) ;
#11103 = CARTESIAN_POINT ( 'NONE',  ( 0.1756481739660004926, -4.720212674039055756, -3.469390959564091492 ) ) ;
#11104 = LINE ( 'NONE', #79, #7390 ) ;
#11105 = EDGE_CURVE ( 'NONE', #16755, #5263, #21522, .T. ) ;
#11106 = CARTESIAN_POINT ( 'NONE',  ( 2.500000000000015543, 1.068589661201712855E-14, -25.03750572909315153 ) ) ;
#11107 = CONICAL_SURFACE ( 'NONE', #14491, 4.750000000000000888, 1.047197551196600074 ) ;
#11108 = DIRECTION ( 'NONE',  ( 0.000000000000000000, 0.7453559924999302311, 0.6666666666666662966 ) ) ;
#11109 = ORIENTED_EDGE ( 'NONE', *, *, #6238, .F. ) ;
#11110 = DIRECTION ( 'NONE',  ( 0.000000000000000000, 0.000000000000000000, 1.000000000000000000 ) ) ;
#11112 = ORIENTED_EDGE ( 'NONE', *, *, #4907, .F. ) ;
#11111 = ORIENTED_EDGE ( 'NONE', *, *, #16944, .T. ) ;
#11113 = EDGE_CURVE ( 'NONE', #9105, #19482, #20378, .T. ) ;
#11114 = ADVANCED_FACE ( 'NONE', ( #19118 ), #13367, .F. ) ;
#11115 = ORIENTED_EDGE ( 'NONE', *, *, #20303, .T. ) ;
#11116 = EDGE_CURVE ( 'NONE', #6445, #13557, #3191, .T. ) ;
#11117 = ADVANCED_FACE ( 'NONE', ( #6547 ), #9724, .F. ) ;
#11118 = AXIS2_PLACEMENT_3D ( 'NONE', #5525, #11270, #4196 ) ;
#11119 = ORIENTED_EDGE ( 'NONE', *, *, #1597, .F. ) ;
#11120 = ORIENTED_EDGE ( 'NONE', *, *, #21542, .F. ) ;
#11121 = VECTOR ( 'NONE', #10562, 1000.000000000000000 ) ;
#11122 = ORIENTED_EDGE ( 'NONE', *, *, #14439, .F. ) ;
#11123 = DIRECTION ( 'NONE',  ( -1.000000000000000000, -4.252453317207022018E-31, 5.551115123125818447E-17 ) ) ;
#11124 = FACE_OUTER_BOUND ( 'NONE', #3659, .T. ) ;
#11125 = ADVANCED_FACE ( 'NONE', ( #4293 ), #13601, .T. ) ;
#11126 = CARTESIAN_POINT ( 'NONE',  ( -2.775557561562891351E-14, 10.74999999999998579, -2.566987298107781257 ) ) ;
#11127 = EDGE_CURVE ( 'NONE', #17658, #6130, #3844, .T. ) ;
#11128 = DIRECTION ( 'NONE',  ( -1.000000000000000000, -2.220446049250314067E-16, 5.825996348268307008E-33 ) ) ;
#11129 = AXIS2_PLACEMENT_3D ( 'NONE', #15469, #15698, #15932 ) ;
#11130 = CARTESIAN_POINT ( 'NONE',  ( -6.999999999999992006, -5.999999999999987566, 6.250000000000005329 ) ) ;
#11131 = CARTESIAN_POINT ( 'NONE',  ( 7.764145988665070774, -12.22513543353773713, 8.011880279048892106 ) ) ;
#11132 = CARTESIAN_POINT ( 'NONE',  ( -89.70000000000057128, -9.020562075079396891E-14, -2.000000000000001776 ) ) ;
#11133 = ADVANCED_FACE ( 'NONE', ( #1019 ), #12116, .T. ) ;
#11134 = CARTESIAN_POINT ( 'NONE',  ( -89.70000000000064233, 5.551115123125782702E-14, -2.000000000000001776 ) ) ;
#11135 = LINE ( 'NONE', #14788, #7478 ) ;
#11136 = CIRCLE ( 'NONE', #15271, 0.4999999999999990563 ) ;
#11137 = B_SPLINE_CURVE_WITH_KNOTS ( 'NONE', 3,
 ( #17318, #1796, #14039, #19800, #19331, #21231, #1450, #19440 ),
 .UNSPECIFIED., .F., .F.,
 ( 4, 2, 2, 4 ),
 ( 0.002775112046897006829, 0.003466237704215410428, 0.004157363361533814895, 0.005539614676170622962 ),
 .UNSPECIFIED. ) ;
#11138 = CARTESIAN_POINT ( 'NONE',  ( 12.84999999999997300, -12.00000000000006928, 4.163336342344337027E-14 ) ) ;
#11139 = PLANE ( 'NONE',  #5512 ) ;
#11140 = VECTOR ( 'NONE', #3018, 1000.000000000000114 ) ;
#11141 = CIRCLE ( 'NONE', #19402, 0.5000000000000028866 ) ;
#11142 =( NAMED_UNIT ( * ) SI_UNIT ( $, .STERADIAN. ) SOLID_ANGLE_UNIT ( ) );
#11143 = LINE ( 'NONE', #18326, #1444 ) ;
#11144 = CYLINDRICAL_SURFACE ( 'NONE', #3656, 0.5000000000000017764 ) ;
#11145 = CIRCLE ( 'NONE', #1758, 0.5000000000000038858 ) ;
#11146 = APPLICATION_CONTEXT ( 'automotive_design' ) ;
#11147 = VERTEX_POINT ( 'NONE', #16987 ) ;
#11148 = CARTESIAN_POINT ( 'NONE',  ( -4.030227849471724966, 38.50929569396286212, -29.00044198939601969 ) ) ;
#11149 = DIRECTION ( 'NONE',  ( 0.000000000000000000, 1.000000000000000000, 0.000000000000000000 ) ) ;
#11150 = VERTEX_POINT ( 'NONE', #8189 ) ;
#11151 = AXIS2_PLACEMENT_3D ( 'NONE', #12189, #17970, #19496 ) ;
#11152 = CARTESIAN_POINT ( 'NONE',  ( 42.00000000000012079, 8.000000000000003553, -12.49999999999999645 ) ) ;
#11153 = EDGE_CURVE ( 'NONE', #19223, #8379, #16997, .T. ) ;
#11154 = LINE ( 'NONE', #22099, #18280 ) ;
#11155 = B_SPLINE_CURVE_WITH_KNOTS ( 'NONE', 3,
 ( #25, #10823, #9061, #19655, #15992, #7085 ),
 .UNSPECIFIED., .F., .F.,
 ( 4, 2, 4 ),
 ( 0.003805860999069545295, 0.004828937044845087005, 0.005852013090620628716 ),
 .UNSPECIFIED. ) ;
#11156 = CARTESIAN_POINT ( 'NONE',  ( 4.030867648405042303, -3.732851566701254953, -0.5345114293579096287 ) ) ;
#11157 = VECTOR ( 'NONE', #8746, 1000.000000000000000 ) ;
#11158 = DIRECTION ( 'NONE',  ( -1.000000000000000000, 0.000000000000000000, 0.000000000000000000 ) ) ;
#11159 = DIRECTION ( 'NONE',  ( 3.885780586188016830E-16, 4.437342591868156373E-31, -1.000000000000000000 ) ) ;
#11160 = CIRCLE ( 'NONE', #17157, 2.800000000000017142 ) ;
#11161 = CARTESIAN_POINT ( 'NONE',  ( -64.00000000000045475, -6.938893903907228378E-14, -2.000000000000001776 ) ) ;
#11162 = FACE_OUTER_BOUND ( 'NONE', #8933, .T. ) ;
#11163 = DIRECTION ( 'NONE',  ( 0.000000000000000000, -1.000000000000000000, 0.000000000000000000 ) ) ;
#11164 = ADVANCED_FACE ( 'NONE', ( #20788 ), #1251, .F. ) ;
#11165 = CARTESIAN_POINT ( 'NONE',  ( 3.000000000291852764, 42.99999999900385461, -18.50000000000000355 ) ) ;
#11166 = CARTESIAN_POINT ( 'NONE',  ( 7.796097383573778572, -13.30002726899557253, 7.943830786858248061 ) ) ;
#11167 = DIRECTION ( 'NONE',  ( -2.013525853228507892E-32, -6.902532920683810383E-31, 1.000000000000000000 ) ) ;
#11168 = DIRECTION ( 'NONE',  ( 1.333893503340774882E-15, 2.778352770573747380E-17, 1.000000000000000000 ) ) ;
#11169 = DIRECTION ( 'NONE',  ( 1.000000000000000000, 0.000000000000000000, 0.000000000000000000 ) ) ;
#11170 = CARTESIAN_POINT ( 'NONE',  ( 10.50000000000000888, -12.50000000000002842, 6.250000000000061284 ) ) ;
#11171 = CARTESIAN_POINT ( 'NONE',  ( 4.071447262713884463, 2.020725942163688504, -3.499999999999999556 ) ) ;
#11172 = VECTOR ( 'NONE', #15600, 1000.000000000000114 ) ;
#11173 = SHAPE_DEFINITION_REPRESENTATION ( #10049, #16280 ) ;
#11174 = ORIENTED_EDGE ( 'NONE', *, *, #20779, .F. ) ;
#11176 = AXIS2_PLACEMENT_3D ( 'NONE', #10347, #4711, #11881 ) ;
#11175 = APPLICATION_CONTEXT ( 'automotive_design' ) ;
#11177 = VECTOR ( 'NONE', #23139, 1000.000000000000000 ) ;
#11178 = AXIS2_PLACEMENT_3D ( 'NONE', #9556, #4482, #11537 ) ;
#11180 = ORIENTED_EDGE ( 'NONE', *, *, #14392, .T. ) ;
#11179 = VERTEX_POINT ( 'NONE', #11471 ) ;
#11181 = FACE_OUTER_BOUND ( 'NONE', #17062, .T. ) ;
#11182 = CARTESIAN_POINT ( 'NONE',  ( 8.160037397871471754, -0.008793114504475355031, 6.662331851011971118 ) ) ;
#11183 = ORIENTED_EDGE ( 'NONE', *, *, #22086, .F. ) ;
#11184 = B_SPLINE_CURVE_WITH_KNOTS ( 'NONE', 3,
 ( #18489, #1903, #18264, #12851, #14848, #21578 ),
 .UNSPECIFIED., .F., .F.,
 ( 4, 2, 4 ),
 ( 0.003358874760055623448, 0.004541967308452153629, 0.005725059856848683376 ),
 .UNSPECIFIED. ) ;
#11185 = CARTESIAN_POINT ( 'NONE',  ( 4.175326769692849993, 4.121399112977843338, -4.212005211934550870E-14 ) ) ;
#11186 = CARTESIAN_POINT ( 'NONE',  ( 36.00000000029184832, 2.999999999003851503, -39.00000000000000000 ) ) ;
#11187 = CARTESIAN_POINT ( 'NONE',  ( 4.082498951862916670, -2.020725942163687616, 3.499999999999999556 ) ) ;
#11188 = TOROIDAL_SURFACE ( 'NONE', #301, 1.000000000000000000, 0.5000000000000000000 ) ;
#11189 = CARTESIAN_POINT ( 'NONE',  ( 42.50000000000020606, 2.499999999999995115, 5.551115123125782702E-14 ) ) ;
#11190 = DIRECTION ( 'NONE',  ( 0.000000000000000000, 0.000000000000000000, 1.000000000000000000 ) ) ;
#11191 = DIRECTION ( 'NONE',  ( 2.775557561562824791E-17, 0.000000000000000000, 1.000000000000000000 ) ) ;
#11192 = DIRECTION ( 'NONE',  ( 1.000000000000000000, 3.469446951953611033E-15, 0.000000000000000000 ) ) ;
#11193 = DIRECTION ( 'NONE',  ( 1.000000000000000000, 0.000000000000000000, 0.000000000000000000 ) ) ;
#11194 = FILL_AREA_STYLE ('',( #6258 ) ) ;
#11195 = FILL_AREA_STYLE ('',( #2256 ) ) ;
#11196 = CARTESIAN_POINT ( 'NONE',  ( 6.000000000291855429, -9.961476088449217059E-10, -3.449999999999997957 ) ) ;
#11197 = CIRCLE ( 'NONE', #18341, 6.000000000000047962 ) ;
#11198 = B_SPLINE_CURVE_WITH_KNOTS ( 'NONE', 3,
 ( #18719, #9781, #16934, #847 ),
 .UNSPECIFIED., .F., .F.,
 ( 4, 4 ),
 ( 2.380739282476591411E-07, 0.002044882221487541018 ),
 .UNSPECIFIED. ) ;
#11199 = DIRECTION ( 'NONE',  ( 1.000000000000000000, -2.168404344971005170E-16, 1.203141491611682442E-30 ) ) ;
#11200 = DIRECTION ( 'NONE',  ( 1.733449886265891589E-32, -4.190823558986610327E-31, 1.000000000000000000 ) ) ;
#11201 = CARTESIAN_POINT ( 'NONE',  ( 7.176407415342007212, -0.3641807091870383761, 8.314790908397654334 ) ) ;
#11202 = ORIENTED_EDGE ( 'NONE', *, *, #16810, .T. ) ;
#11203 = EDGE_CURVE ( 'NONE', #16719, #5817, #11828, .T. ) ;
#11204 =( NAMED_UNIT ( * ) PLANE_ANGLE_UNIT ( ) SI_UNIT ( $, .RADIAN. ) );
#11206 = EDGE_LOOP ( 'NONE', ( #14853, #14937, #7734, #5849 ) ) ;
#11205 = ORIENTED_EDGE ( 'NONE', *, *, #19140, .F. ) ;
#11207 = UNCERTAINTY_MEASURE_WITH_UNIT (LENGTH_MEASURE( 1.000000000000000082E-05 ), #17292, 'distance_accuracy_value', 'NONE');
#11208 = AXIS2_PLACEMENT_3D ( 'NONE', #4593, #11776, #10021 ) ;
#11209 = ORIENTED_EDGE ( 'NONE', *, *, #7371, .T. ) ;
#11210 = ORIENTED_EDGE ( 'NONE', *, *, #597, .T. ) ;
#11212 = ORIENTED_EDGE ( 'NONE', *, *, #11070, .T. ) ;
#11211 = ORIENTED_EDGE ( 'NONE', *, *, #16419, .T. ) ;
#11213 = ORIENTED_EDGE ( 'NONE', *, *, #7394, .F. ) ;
#11214 = DIRECTION ( 'NONE',  ( 0.000000000000000000, 0.000000000000000000, 1.000000000000000000 ) ) ;
#11215 = ORIENTED_EDGE ( 'NONE', *, *, #19209, .F. ) ;
#11216 = ORIENTED_EDGE ( 'NONE', *, *, #19285, .F. ) ;
#11217 = CARTESIAN_POINT ( 'NONE',  ( 4.000000000000003553, 2.309401076758525573, -0.3572655899081733644 ) ) ;
#11218 = CIRCLE ( 'NONE', #11579, 0.5000000000000004441 ) ;
#11219 = AXIS2_PLACEMENT_3D ( 'NONE', #1397, #19508, #8808 ) ;
#11220 = VECTOR ( 'NONE', #4621, 1000.000000000000000 ) ;
#11221 = FACE_OUTER_BOUND ( 'NONE', #12232, .T. ) ;
#11222 = FACE_OUTER_BOUND ( 'NONE', #4524, .T. ) ;
#11223 = CARTESIAN_POINT ( 'NONE',  ( 0.000000000000000000, 0.000000000000000000, 0.000000000000000000 ) ) ;
#11224 = CARTESIAN_POINT ( 'NONE',  ( 2.918498775983380256E-10, 2.999999999003851503, -45.00000000000000000 ) ) ;
#11225 = CARTESIAN_POINT ( 'NONE',  ( 77.42435809754140053, -10.99999999999981526, -6.499999999999999112 ) ) ;
#11226 = LINE ( 'NONE', #9351, #3889 ) ;
#11227 = FACE_OUTER_BOUND ( 'NONE', #14623, .T. ) ;
#11228 = EDGE_CURVE ( 'NONE', #9098, #1910, #1242, .T. ) ;
#11229 = CARTESIAN_POINT ( 'NONE',  ( -4.330127018922248716, 4.689110867544532546, 7.500000000000007105 ) ) ;
#11230 = CIRCLE ( 'NONE', #2211, 4.750000000000000000 ) ;
#11231 = CARTESIAN_POINT ( 'NONE',  ( 37.43301270189239460, 10.75000000000000178, -2.999999999999959144 ) ) ;
#11232 = ORIENTED_EDGE ( 'NONE', *, *, #4707, .T. ) ;
#11233 = EDGE_CURVE ( 'NONE', #4291, #6467, #4596, .T. ) ;
#11234 = AXIS2_PLACEMENT_3D ( 'NONE', #16289, #3818, #10994 ) ;
#11235 = CARTESIAN_POINT ( 'NONE',  ( 5.484827557301452217, -1.325747111984059590, 0.000000000000000000 ) ) ;
#11237 = EDGE_LOOP ( 'NONE', ( #22122, #17896, #9023 ) ) ;
#11236 = ORIENTED_EDGE ( 'NONE', *, *, #10802, .F. ) ;
#11238 = ORIENTED_EDGE ( 'NONE', *, *, #7501, .F. ) ;
#11239 = EDGE_CURVE ( 'NONE', #23201, #7712, #2536, .T. ) ;
#11240 = ORIENTED_EDGE ( 'NONE', *, *, #8114, .T. ) ;
#11241 = EDGE_CURVE ( 'NONE', #20509, #1546, #21533, .T. ) ;
#11242 = EDGE_CURVE ( 'NONE', #15365, #15655, #4875, .T. ) ;
#11243 = CARTESIAN_POINT ( 'NONE',  ( 36.00000000029184832, 2.999999999003851503, -18.50000000000000355 ) ) ;
#11244 = CYLINDRICAL_SURFACE ( 'NONE', #23023, 3.999999999999994671 ) ;
#11245 = FACE_OUTER_BOUND ( 'NONE', #3361, .T. ) ;
#11246 = AXIS2_PLACEMENT_3D ( 'NONE', #22979, #3335, #17667 ) ;
#11247 = CARTESIAN_POINT ( 'NONE',  ( 0.000000000000000000, 1.387778780781445676E-14, 17.24999999999997513 ) ) ;
#11248 = DIRECTION ( 'NONE',  ( 1.066194817212773768E-26, 0.000000000000000000, 1.000000000000000000 ) ) ;
#11249 = DIRECTION ( 'NONE',  ( -5.551115123561405253E-17, -1.000000000000000000, -2.256980353643891447E-27 ) ) ;
#11250 = CARTESIAN_POINT ( 'NONE',  ( -7.725871784772736284, -12.18565941508500394, 8.100883686805090633 ) ) ;
#11251 = ADVANCED_FACE ( 'NONE', ( #21009 ), #6889, .T. ) ;
#11252 = EDGE_CURVE ( 'NONE', #16622, #22329, #5247, .T. ) ;
#11253 = CARTESIAN_POINT ( 'NONE',  ( 63.53596085922836068, -2.925414806476678287, 6.500000000000123457 ) ) ;
#11254 = CARTESIAN_POINT ( 'NONE',  ( 1.387778780781446070E-15, 3.061616997868387579E-16, -2.500000000000001332 ) ) ;
#11255 = AXIS2_PLACEMENT_3D ( 'NONE', #17104, #11159, #13165 ) ;
#11256 = CARTESIAN_POINT ( 'NONE',  ( -50.65685424949274562, -2.700000000000125855, 8.000000000000062172 ) ) ;
#11257 = DIRECTION ( 'NONE',  ( 1.000000000000000000, -1.847414967615758933E-47, 3.885780586188017323E-16 ) ) ;
#11258 = AXIS2_PLACEMENT_3D ( 'NONE', #20962, #17957, #9126 ) ;
#11259 = DIRECTION ( 'NONE',  ( 1.000000000000000000, 0.000000000000000000, 0.000000000000000000 ) ) ;
#11260 = PLANE ( 'NONE',  #5165 ) ;
#11261 = ADVANCED_FACE ( 'NONE', ( #10293 ), #21909, .T. ) ;
#11262 = ADVANCED_FACE ( 'NONE', ( #17466 ), #1474, .T. ) ;
#11263 = ORIENTED_EDGE ( 'NONE', *, *, #10616, .T. ) ;
#11264 = EDGE_CURVE ( 'NONE', #7097, #1072, #17461, .T. ) ;
#11265 = DIRECTION ( 'NONE',  ( -0.6819983600625064701, -0.7313537016191632434, 0.000000000000000000 ) ) ;
#11266 = LINE ( 'NONE', #13158, #16209 ) ;
#11267 = ORIENTED_EDGE ( 'NONE', *, *, #17147, .T. ) ;
#11268 = AXIS2_PLACEMENT_3D ( 'NONE', #2158, #14637, #18179 ) ;
#11269 = DIRECTION ( 'NONE',  ( 0.000000000000000000, 1.000000000000000000, 0.000000000000000000 ) ) ;
#11270 = DIRECTION ( 'NONE',  ( -1.000000000000000000, -3.254448077276381206E-32, -1.066788928082016908E-26 ) ) ;
#11271 = LINE ( 'NONE', #13388, #19226 ) ;
#11272 = CARTESIAN_POINT ( 'NONE',  ( 2.023222897811621159E-14, -0.3420925509381568808, -3.500000000000033751 ) ) ;
#11273 = CARTESIAN_POINT ( 'NONE',  ( 54.42435809754113052, -4.000000000000003553, -6.499999999999999112 ) ) ;
#11274 = CARTESIAN_POINT ( 'NONE',  ( -4.211140560182305315, -2.431303136016589761, -3.745885042887437510 ) ) ;
#11275 = PLANE ( 'NONE',  #6441 ) ;
#11276 = DIRECTION ( 'NONE',  ( 1.000000000000000000, 0.000000000000000000, 0.000000000000000000 ) ) ;
#11277 = CARTESIAN_POINT ( 'NONE',  ( 0.000000000000000000, 0.000000000000000000, -0.2800830152838822418 ) ) ;
#11278 = CARTESIAN_POINT ( 'NONE',  ( 63.19496167919701435, -3.291091657286332683, -6.499999999999970690 ) ) ;
#11279 = CARTESIAN_POINT ( 'NONE',  ( 3.948103430091022492, 2.682758828852624067, -2.353325403973583807 ) ) ;
#11280 = CARTESIAN_POINT ( 'NONE',  ( 124.5000000000019469, -13.52760560296373171, -6.938893903907228378E-15 ) ) ;
#11281 =( LENGTH_UNIT ( ) NAMED_UNIT ( * ) SI_UNIT ( .MILLI., .METRE. ) );
#11282 = CARTESIAN_POINT ( 'NONE',  ( 4.158806965674304301, -1.986429158307097431, -3.559403772175838476 ) ) ;
#11283 = CIRCLE ( 'NONE', #3759, 2.999999999999995559 ) ;
#11284 = EDGE_CURVE ( 'NONE', #15739, #12056, #20399, .T. ) ;
#11285 = PRODUCT_CONTEXT ( 'NONE', #11175, 'mechanical' ) ;
#11286 = ORIENTED_EDGE ( 'NONE', *, *, #8247, .T. ) ;
#11287 = EDGE_CURVE ( 'NONE', #1883, #6815, #4220, .T. ) ;
#11289 = ORIENTED_EDGE ( 'NONE', *, *, #23179, .F. ) ;
#11288 = ORIENTED_EDGE ( 'NONE', *, *, #21206, .F. ) ;
#11290 = CARTESIAN_POINT ( 'NONE',  ( 0.4500000002918510544, 42.99999999900385461, -26.00000000000000000 ) ) ;
#11291 = DIRECTION ( 'NONE',  ( 0.000000000000000000, -1.000000000000000000, 0.000000000000000000 ) ) ;
#11292 = DIRECTION ( 'NONE',  ( 1.550910762415566494E-16, 1.000000000000000000, -8.135128085091684243E-31 ) ) ;
#11293 = ORIENTED_EDGE ( 'NONE', *, *, #7548, .F. ) ;
#11294 = CIRCLE ( 'NONE', #3050, 4.500000000000000888 ) ;
#11295 = CARTESIAN_POINT ( 'NONE',  ( -2.700000000000119194, -2.000000000000001776, -8.000000000000007105 ) ) ;
#11296 = DIRECTION ( 'NONE',  ( 1.066786462891689527E-26, 6.656013887802287108E-31, 1.000000000000000000 ) ) ;
#11297 = DIRECTION ( 'NONE',  ( -6.938893903907259932E-15, 1.000000000000000000, 1.553069907153866992E-30 ) ) ;
#11298 = CARTESIAN_POINT ( 'NONE',  ( 86.02937988905577527, -9.453020409440155092, -5.999999999999991118 ) ) ;
#11299 = CARTESIAN_POINT ( 'NONE',  ( 77.42435809754137210, -6.999999999999811706, 6.000000000000088818 ) ) ;
#11300 = CARTESIAN_POINT ( 'NONE',  ( 2.499999999999998668, 2.000000000000001776, -17.50000000000000711 ) ) ;
#11301 = LINE ( 'NONE', #7776, #20846 ) ;
#11302 = PRESENTATION_STYLE_ASSIGNMENT (( #9779 ) ) ;
#11303 = CARTESIAN_POINT ( 'NONE',  ( 10.50000000000000888, 0.000000000000000000, 9.249999999999980460 ) ) ;
#11304 = FILL_AREA_STYLE_COLOUR ( '', #17964 ) ;
#11305 = CARTESIAN_POINT ( 'NONE',  ( 37.86602540378466841, 0.000000000000000000, -6.499999999999992006 ) ) ;
#11306 = DIRECTION ( 'NONE',  ( -1.000000000000000000, 4.190823558986610327E-31, -1.733449886265890494E-32 ) ) ;
#11307 = ADVANCED_FACE ( 'NONE', ( #8885 ), #13828, .F. ) ;
#11308 = ORIENTED_EDGE ( 'NONE', *, *, #2498, .T. ) ;
#11309 = AXIS2_PLACEMENT_3D ( 'NONE', #12070, #4904, #15837 ) ;
#11310 = CIRCLE ( 'NONE', #7203, 7.500000000000001776 ) ;
#11312 = ORIENTED_EDGE ( 'NONE', *, *, #20020, .F. ) ;
#11311 = EDGE_LOOP ( 'NONE', ( #13528, #6271, #3432, #860 ) ) ;
#11313 = ADVANCED_FACE ( 'NONE', ( #23132 ), #15873, .T. ) ;
#11314 = ORIENTED_EDGE ( 'NONE', *, *, #7822, .F. ) ;
#11316 = ORIENTED_EDGE ( 'NONE', *, *, #6078, .F. ) ;
#11315 = ORIENTED_EDGE ( 'NONE', *, *, #22967, .T. ) ;
#11317 = VERTEX_POINT ( 'NONE', #19583 ) ;
#11318 = CARTESIAN_POINT ( 'NONE',  ( 30.60000000000000142, 2.775557561562891351E-14, -2.081668171172168513E-14 ) ) ;
#11319 = VERTEX_POINT ( 'NONE', #23252 ) ;
#11320 = ORIENTED_EDGE ( 'NONE', *, *, #13548, .F. ) ;
#11321 = CARTESIAN_POINT ( 'NONE',  ( 1.015987785799958376E-14, -3.202582148906756299, -1.452965002680425277 ) ) ;
#11322 = DIRECTION ( 'NONE',  ( -1.000000000000000000, 1.276756478318922725E-15, -1.333893503340766402E-15 ) ) ;
#11323 = CARTESIAN_POINT ( 'NONE',  ( -7.120027569165166881, -2.450222941140165922, 8.099087005775098547 ) ) ;
#11324 = EDGE_CURVE ( 'NONE', #8293, #6969, #17695, .T. ) ;
#11325 = CARTESIAN_POINT ( 'NONE',  ( 0.000000000000000000, 3.031088913245508110, -1.750000000000029310 ) ) ;
#11326 = DIRECTION ( 'NONE',  ( 0.6819983600624981435, -0.7313537016191709039, 0.000000000000000000 ) ) ;
#11327 = CONICAL_SURFACE ( 'NONE', #2317, 12.50000000000003375, 0.1651486774146268266 ) ;
#11328 = CIRCLE ( 'NONE', #2687, 6.999999999999999112 ) ;
#11329 = CARTESIAN_POINT ( 'NONE',  ( -95.20000000000065654, 6.938893903907228378E-15, -2.000000000000001776 ) ) ;
#11330 = DIRECTION ( 'NONE',  ( 1.000000000000000000, 1.734723475976805517E-15, 0.000000000000000000 ) ) ;
#11331 = DIRECTION ( 'NONE',  ( -0.7071067811865532349, 0.7071067811865416886, 1.565905175853764455E-16 ) ) ;
#11332 = CARTESIAN_POINT ( 'NONE',  ( 82.19834661797897013, -5.880524088665628923, 6.000000000000109246 ) ) ;
#11333 = ORIENTED_EDGE ( 'NONE', *, *, #20656, .F. ) ;
#11334 = VECTOR ( 'NONE', #8163, 1000.000000000000000 ) ;
#11335 = CARTESIAN_POINT ( 'NONE',  ( 12.84999999999997300, -14.00000000000008882, -2.549999999999945199 ) ) ;
#11337 = ORIENTED_EDGE ( 'NONE', *, *, #19558, .T. ) ;
#11336 = ORIENTED_EDGE ( 'NONE', *, *, #18183, .T. ) ;
#11338 = ORIENTED_EDGE ( 'NONE', *, *, #2930, .T. ) ;
#11339 = ORIENTED_EDGE ( 'NONE', *, *, #20909, .F. ) ;
#11340 = CIRCLE ( 'NONE', #23000, 6.500000000000061284 ) ;
#11341 = EDGE_LOOP ( 'NONE', ( #11837, #18127, #21356, #15880 ) ) ;
#11342 = AXIS2_PLACEMENT_3D ( 'NONE', #11247, #13139, #16308 ) ;
#11343 = VERTEX_POINT ( 'NONE', #8535 ) ;
#11344 = CARTESIAN_POINT ( 'NONE',  ( -3.999999999708153453, 38.99999999900385461, -15.99999999999999289 ) ) ;
#11345 = DIRECTION ( 'NONE',  ( 0.000000000000000000, 3.469446951953618922E-15, 1.000000000000000000 ) ) ;
#11346 = ORIENTED_EDGE ( 'NONE', *, *, #18713, .T. ) ;
#11347 = DIRECTION ( 'NONE',  ( -3.885780586188016830E-16, -4.437342591868156373E-31, 1.000000000000000000 ) ) ;
#11348 = EDGE_CURVE ( 'NONE', #11578, #20045, #17755, .T. ) ;
#11349 = CIRCLE ( 'NONE', #3848, 2.499999999999993339 ) ;
#11350 = DIRECTION ( 'NONE',  ( -1.000000000000000000, 2.818925648462279658E-14, 0.000000000000000000 ) ) ;
#11351 = CARTESIAN_POINT ( 'NONE',  ( 12.84999999999997300, -1.500000000000001332, 5.750000000000005329 ) ) ;
#11352 = DIRECTION ( 'NONE',  ( -0.000000000000000000, -1.000000000000000000, -0.000000000000000000 ) ) ;
#11353 = CARTESIAN_POINT ( 'NONE',  ( -7.551224464536113068, -11.87866898603341070, 7.234820221745398960 ) ) ;
#11354 = DIRECTION ( 'NONE',  ( -5.551115123125796261E-17, 2.869019762633796499E-16, 1.000000000000000000 ) ) ;
#11355 = ADVANCED_FACE ( 'NONE', ( #6766 ), #11753, .T. ) ;
#11356 = AXIS2_PLACEMENT_3D ( 'NONE', #12633, #17827, #23251 ) ;
#11357 = CARTESIAN_POINT ( 'NONE',  ( 8.113551354210041922, -1.583389928980787120, 7.426820295479616973 ) ) ;
#11358 = VECTOR ( 'NONE', #20198, 1000.000000000000000 ) ;
#11360 = EDGE_CURVE ( 'NONE', #14190, #11003, #21689, .T. ) ;
#11359 = CARTESIAN_POINT ( 'NONE',  ( -10.49999999999995381, -1.499999999999997780, 6.250000000000019540 ) ) ;
#11361 = AXIS2_PLACEMENT_3D ( 'NONE', #22775, #4533, #789 ) ;
#11362 = AXIS2_PLACEMENT_3D ( 'NONE', #8211, #13621, #11608 ) ;
#11363 = FACE_OUTER_BOUND ( 'NONE', #6242, .T. ) ;
#11364 = CARTESIAN_POINT ( 'NONE',  ( 0.000000000000000000, 0.000000000000000000, 3.499999999999999556 ) ) ;
#11365 = EDGE_LOOP ( 'NONE', ( #6730, #8382, #20971 ) ) ;
#11366 = ORIENTED_EDGE ( 'NONE', *, *, #50, .F. ) ;
#11367 = ORIENTED_EDGE ( 'NONE', *, *, #16881, .F. ) ;
#11368 = CARTESIAN_POINT ( 'NONE',  ( -12.85000000000002807, -1.999999999999998224, 6.249999999999950262 ) ) ;
#11369 = EDGE_CURVE ( 'NONE', #19811, #7132, #21979, .T. ) ;
#11370 = EDGE_CURVE ( 'NONE', #1330, #7794, #14094, .T. ) ;
#11371 = DIRECTION ( 'NONE',  ( 1.000000000000000000, -1.276756478318923119E-15, 1.403805528459192781E-15 ) ) ;
#11372 = VECTOR ( 'NONE', #9008, 1000.000000000000000 ) ;
#11373 = VECTOR ( 'NONE', #14814, 1000.000000000000000 ) ;
#11374 = EDGE_LOOP ( 'NONE', ( #12773, #22759, #1128, #12412 ) ) ;
#11375 = AXIS2_PLACEMENT_3D ( 'NONE', #7437, #14606, #20133 ) ;
#11376 = B_SPLINE_CURVE_WITH_KNOTS ( 'NONE', 3,
 ( #281, #19139, #19251, #14082 ),
 .UNSPECIFIED., .F., .F.,
 ( 4, 4 ),
 ( 2.380735702043565917E-07, 0.002775112046897006395 ),
 .UNSPECIFIED. ) ;
#11377 = CARTESIAN_POINT ( 'NONE',  ( 37.86602540378461157, 11.00000000000000000, -10.86602540378450676 ) ) ;
#11378 = CIRCLE ( 'NONE', #22274, 0.4999999999999994449 ) ;
#11379 = AXIS2_PLACEMENT_3D ( 'NONE', #17551, #13913, #7111 ) ;
#11380 = FACE_OUTER_BOUND ( 'NONE', #829, .T. ) ;
#11381 = FACE_OUTER_BOUND ( 'NONE', #15821, .T. ) ;
#11383 = EDGE_CURVE ( 'NONE', #7568, #21501, #2738, .T. ) ;
#11382 = AXIS2_PLACEMENT_3D ( 'NONE', #18027, #5084, #15773 ) ;
#11384 = CYLINDRICAL_SURFACE ( 'NONE', #16646, 2.550000000000012701 ) ;
#11385 = CARTESIAN_POINT ( 'NONE',  ( 25.15499999999999403, 0.000000000000000000, -6.938893903907228378E-15 ) ) ;
#11386 = DIRECTION ( 'NONE',  ( -1.000000000000000000, 1.387778780781436209E-14, -1.404432126150814819E-14 ) ) ;
#11387 = CARTESIAN_POINT ( 'NONE',  ( 2.775557561562891351E-14, 2.499999999999995115, -12.99999999999999822 ) ) ;
#11388 = CARTESIAN_POINT ( 'NONE',  ( 7.499999999999984013, -13.02884243125068764, 9.522727272727365744 ) ) ;
#11389 = CARTESIAN_POINT ( 'NONE',  ( 22.49999999999992539, 1.999999999999960032, -18.75000000000001421 ) ) ;
#11390 = EDGE_CURVE ( 'NONE', #9452, #16835, #18064, .T. ) ;
#11391 = ADVANCED_FACE ( 'NONE', ( #7581 ), #20290, .T. ) ;
#11392 = CARTESIAN_POINT ( 'NONE',  ( -8.326672684688674053E-14, -1.999999999999988010, -7.500000000000034639 ) ) ;
#11393 = DIRECTION ( 'NONE',  ( -5.551115123561405253E-17, -1.000000000000000000, -2.256980353643891447E-27 ) ) ;
#11395 = EDGE_CURVE ( 'NONE', #15946, #18765, #18149, .T. ) ;
#11394 = CARTESIAN_POINT ( 'NONE',  ( -6.000000000000074607, 4.799999999999964295, 7.500000000000062172 ) ) ;
#11396 = CIRCLE ( 'NONE', #14417, 4.749999999999986677 ) ;
#11397 = CARTESIAN_POINT ( 'NONE',  ( 4.151274195509686571, 2.039912954708743786, -3.533232880573500712 ) ) ;
#11398 = AXIS2_PLACEMENT_3D ( 'NONE', #2331, #2451, #21990 ) ;
#11399 = AXIS2_PLACEMENT_3D ( 'NONE', #11490, #15488, #2559 ) ;
#11400 = VECTOR ( 'NONE', #3530, 1000.000000000000000 ) ;
#11401 = ORIENTED_EDGE ( 'NONE', *, *, #12335, .F. ) ;
#11402 = EDGE_CURVE ( 'NONE', #17530, #13979, #3121, .T. ) ;
#11403 = EDGE_CURVE ( 'NONE', #18644, #7880, #291, .T. ) ;
#11405 = ORIENTED_EDGE ( 'NONE', *, *, #4332, .F. ) ;
#11404 = ORIENTED_EDGE ( 'NONE', *, *, #11233, .F. ) ;
#11406 = DIRECTION ( 'NONE',  ( 1.066786462891689527E-26, 6.656013887802287108E-31, 1.000000000000000000 ) ) ;
#11407 = CARTESIAN_POINT ( 'NONE',  ( 0.4637351969133413077, -1.749999999999980904, -4.750000000000023981 ) ) ;
#11408 = CARTESIAN_POINT ( 'NONE',  ( -4.499999999708154341, 36.49999999900384751, -26.00000000000000000 ) ) ;
#11409 = CIRCLE ( 'NONE', #11028, 0.5000000000000038858 ) ;
#11410 = ORIENTED_EDGE ( 'NONE', *, *, #22014, .T. ) ;
#11411 = CIRCLE ( 'NONE', #13308, 0.5000000000000004441 ) ;
#11412 = DIRECTION ( 'NONE',  ( -0.000000000000000000, 1.000000000000000000, 0.000000000000000000 ) ) ;
#11413 = ADVANCED_FACE ( 'NONE', ( #5598 ), #7471, .T. ) ;
#11414 = CARTESIAN_POINT ( 'NONE',  ( -2.500000000000015543, 1.737584070339862599E-14, -25.03750572909315864 ) ) ;
#11415 = AXIS2_PLACEMENT_3D ( 'NONE', #19112, #17224, #6190 ) ;
#11416 = DIRECTION ( 'NONE',  ( 0.7071067811865460184, -0.7071067811865490160, -1.010793663541200360E-16 ) ) ;
#11417 = CARTESIAN_POINT ( 'NONE',  ( -6.649675532656707411, 36.01889503913411517, -17.57202100271285872 ) ) ;
#11418 = DIRECTION ( 'NONE',  ( 1.454462294001240516E-30, 1.000000000000000000, 0.000000000000000000 ) ) ;
#11419 = EDGE_CURVE ( 'NONE', #20589, #20148, #21824, .T. ) ;
#11420 = CARTESIAN_POINT ( 'NONE',  ( 0.000000000000000000, 3.031088913245536087, 1.749999999999998002 ) ) ;
#11421 = CARTESIAN_POINT ( 'NONE',  ( 6.500000000000339284, 0.5000000000001947331, 6.500000000000130562 ) ) ;
#11422 = CARTESIAN_POINT ( 'NONE',  ( 4.175813232069142344, -4.122719923832743660, 0.000000000000000000 ) ) ;
#11423 =( LENGTH_UNIT ( ) NAMED_UNIT ( * ) SI_UNIT ( .MILLI., .METRE. ) );
#11424 = DIRECTION ( 'NONE',  ( -1.000000000000000000, -4.252453317207022018E-31, 5.551115123125818447E-17 ) ) ;
#11425 = CARTESIAN_POINT ( 'NONE',  ( -12.84999999999999964, -12.00000000000011191, -5.749999999999963585 ) ) ;
#11426 = CARTESIAN_POINT ( 'NONE',  ( 3.469446951953614189E-15, 1.500000000000015099, -19.00000000000001066 ) ) ;
#11427 = DIRECTION ( 'NONE',  ( 0.000000000000000000, 0.000000000000000000, 1.000000000000000000 ) ) ;
#11428 = ORIENTED_EDGE ( 'NONE', *, *, #10672, .T. ) ;
#11429 = AXIS2_PLACEMENT_3D ( 'NONE', #22514, #2982, #17549 ) ;
#11430 = CIRCLE ( 'NONE', #7322, 0.5000000000000029976 ) ;
#11432 = VERTEX_POINT ( 'NONE', #9461 ) ;
#11431 = ORIENTED_EDGE ( 'NONE', *, *, #7673, .T. ) ;
#11433 = EDGE_LOOP ( 'NONE', ( #21693, #2184 ) ) ;
#11435 = VERTEX_POINT ( 'NONE', #12874 ) ;
#11434 = ORIENTED_EDGE ( 'NONE', *, *, #12969, .F. ) ;
#11436 = ORIENTED_EDGE ( 'NONE', *, *, #18893, .T. ) ;
#11437 = CARTESIAN_POINT ( 'NONE',  ( 5.551115123125782702E-14, 5.499999999999980460, 2.500000000000071498 ) ) ;
#11438 = CARTESIAN_POINT ( 'NONE',  ( -50.65685424949281668, 0.5000000000000143219, 7.500000000000034639 ) ) ;
#11439 = ORIENTED_EDGE ( 'NONE', *, *, #14707, .T. ) ;
#11440 = CARTESIAN_POINT ( 'NONE',  ( 54.42435809754113052, -4.000000000000003553, -6.000000000000012434 ) ) ;
#11441 = FACE_OUTER_BOUND ( 'NONE', #854, .T. ) ;
#11442 = ADVANCED_FACE ( 'NONE', ( #5835 ), #20057, .F. ) ;
#11443 = DIRECTION ( 'NONE',  ( 0.000000000000000000, 0.000000000000000000, 1.000000000000000000 ) ) ;
#11444 = DIRECTION ( 'NONE',  ( -9.693522803355793065E-26, 5.963788443470849249E-28, 1.000000000000000000 ) ) ;
#11445 = AXIS2_PLACEMENT_3D ( 'NONE', #18831, #11644, #13775 ) ;
#11446 = DIRECTION ( 'NONE',  ( -1.000000000000000000, 0.000000000000000000, 0.000000000000000000 ) ) ;
#11447 = AXIS2_PLACEMENT_3D ( 'NONE', #4955, #10600, #14259 ) ;
#11448 = CARTESIAN_POINT ( 'NONE',  ( 7.521298409251896189, -2.242072331701569166, 8.817899680514919680 ) ) ;
#11449 = CARTESIAN_POINT ( 'NONE',  ( 4.033906725094494661, -1.419670120619062503, 3.499999999999970246 ) ) ;
#11450 = CARTESIAN_POINT ( 'NONE',  ( 59.19834661797874986, 1.119475911334072427, -5.999999999999908518 ) ) ;
#11451 = ADVANCED_FACE ( 'NONE', ( #21943 ), #4043, .F. ) ;
#11452 = CARTESIAN_POINT ( 'NONE',  ( 6.938893903907228378E-15, 4.618802153517023612, -5.000000000000000888 ) ) ;
#11453 = PLANE ( 'NONE',  #7790 ) ;
#11454 = CARTESIAN_POINT ( 'NONE',  ( -4.920724633012840243, 13.68667664578917709, -28.86177711096811649 ) ) ;
#11455 = LINE ( 'NONE', #20410, #2879 ) ;
#11456 = EDGE_CURVE ( 'NONE', #9368, #7127, #8159, .T. ) ;
#11457 = VERTEX_POINT ( 'NONE', #11798 ) ;
#11458 =( NAMED_UNIT ( * ) PLANE_ANGLE_UNIT ( ) SI_UNIT ( $, .RADIAN. ) );
#11460 = ORIENTED_EDGE ( 'NONE', *, *, #12932, .T. ) ;
#11459 = ORIENTED_EDGE ( 'NONE', *, *, #778, .T. ) ;
#11461 = ORIENTED_EDGE ( 'NONE', *, *, #21191, .F. ) ;
#11462 = AXIS2_PLACEMENT_3D ( 'NONE', #4560, #20932, #4800 ) ;
#11463 = ORIENTED_EDGE ( 'NONE', *, *, #10188, .F. ) ;
#11464 = VERTEX_POINT ( 'NONE', #13458 ) ;
#11465 = EDGE_LOOP ( 'NONE', ( #4138, #9955 ) ) ;
#11466 = DIRECTION ( 'NONE',  ( -0.7313537016191767881, -0.6819983600624918152, -4.403559511741033569E-16 ) ) ;
#11467 = FACE_OUTER_BOUND ( 'NONE', #11781, .T. ) ;
#11468 = ORIENTED_EDGE ( 'NONE', *, *, #22541, .F. ) ;
#11469 = DIRECTION ( 'NONE',  ( 0.000000000000000000, -1.000000000000000000, 0.000000000000000000 ) ) ;
#11470 =( BOUNDED_SURFACE ( )  B_SPLINE_SURFACE ( 3, 2, ( 
 ( #20208, #11018, #13143 ),
 ( #7497, #4075, #12785 ),
 ( #18430, #2307, #9488 ),
 ( #16418, #21631, #5506 ),
 ( #16651, #563, #20318 ),
 ( #4181, #9152, #9729 ),
 ( #13371, #15120, #20674 ),
 ( #22547, #2660, #2542 ),
 ( #20794, #2781, #6432 ),
 ( #15231, #11594, #1143 ),
 ( #13251, #1023, #794 ),
 ( #19122, #4661, #4298 ),
 ( #16883, #9963, #4538 ),
 ( #15009, #18657, #6201 ) ),
 .UNSPECIFIED., .F., .F., .F. ) 
 B_SPLINE_SURFACE_WITH_KNOTS ( ( 4, 2, 2, 2, 2, 2, 4 ),
 ( 3, 3 ),
 ( 0.000000000000000000, 0.0009385527998839224935, 0.001407829199825883686, 0.001877105599767844987, 0.002346381999709806071, 0.002815658399651767372, 0.003754211199535689974 ),
 ( 0.000000000000000000, 1.000000000000000000 ),
 .UNSPECIFIED. ) 
 GEOMETRIC_REPRESENTATION_ITEM ( )  RATIONAL_B_SPLINE_SURFACE ( (
 ( 1.000000000000000000, 0.7071067811865459074, 1.000000000000000000),
 ( 1.000000000000000000, 0.7217349950158724603, 1.000000000000000000),
 ( 1.000000000000000000, 0.7325631490737404272, 1.000000000000000000),
 ( 1.000000000000000000, 0.7426392126583049036, 1.000000000000000000),
 ( 1.000000000000000000, 0.7449451721693781669, 1.000000000000000000),
 ( 1.000000000000000000, 0.7474053618998787174, 1.000000000000000000),
 ( 1.000000000000000000, 0.7475947887410587800, 1.000000000000000000),
 ( 1.000000000000000000, 0.7461109904165237339, 1.000000000000000000),
 ( 1.000000000000000000, 0.7444113185331598936, 1.000000000000000000),
 ( 1.000000000000000000, 0.7395217850811542926, 1.000000000000000000),
 ( 1.000000000000000000, 0.7363545993504476694, 1.000000000000000000),
 ( 1.000000000000000000, 0.7253814056384388920, 1.000000000000000000),
 ( 1.000000000000000000, 0.7159765610437544003, 1.000000000000000000),
 ( 1.000000000000000000, 0.7071067811865461294, 1.000000000000000000) ) ) 
 REPRESENTATION_ITEM ( '' )  SURFACE ( )  );
#11471 = CARTESIAN_POINT ( 'NONE',  ( 3.674234614174737068, 0.7500000000000492939, -3.000000000000002665 ) ) ;
#11472 = CARTESIAN_POINT ( 'NONE',  ( -2.081668171172168513E-14, 4.250000000000003553, -0.2500000000000002220 ) ) ;
#11473 = FACE_OUTER_BOUND ( 'NONE', #5288, .T. ) ;
#11474 = CARTESIAN_POINT ( 'NONE',  ( 4.114405500665259119, 4.051151509359430136, -4.376560574388856425E-17 ) ) ;
#11475 = DIRECTION ( 'NONE',  ( -0.000000000000000000, -1.000000000000000000, -0.000000000000000000 ) ) ;
#11476 = DIRECTION ( 'NONE',  ( 3.070652698126929572E-17, 1.000000000000000000, -2.869019762633796499E-16 ) ) ;
#11477 = DIRECTION ( 'NONE',  ( 1.927470528863118556E-16, 1.000000000000000000, 0.000000000000000000 ) ) ;
#11478 = CARTESIAN_POINT ( 'NONE',  ( 0.2499999999999794054, 1.500000000000015099, -2.000000000000001776 ) ) ;
#11479 = SURFACE_STYLE_FILL_AREA ( #7618 ) ;
#11480 = FACE_OUTER_BOUND ( 'NONE', #11488, .T. ) ;
#11481 = CARTESIAN_POINT ( 'NONE',  ( 4.630153689607046985, 6.577590292450076941E-16, 5.371010071662833063 ) ) ;
#11482 = EDGE_LOOP ( 'NONE', ( #23002, #801, #21391, #22876 ) ) ;
#11483 = AXIS2_PLACEMENT_3D ( 'NONE', #1172, #4806, #4696 ) ;
#11484 = EDGE_CURVE ( 'NONE', #5612, #17281, #2742, .T. ) ;
#11485 = ORIENTED_EDGE ( 'NONE', *, *, #20917, .T. ) ;
#11486 = ORIENTED_EDGE ( 'NONE', *, *, #303, .T. ) ;
#11487 = ORIENTED_EDGE ( 'NONE', *, *, #3866, .T. ) ;
#11488 = EDGE_LOOP ( 'NONE', ( #1768, #2873, #18158, #14828 ) ) ;
#11489 = DIRECTION ( 'NONE',  ( 5.551115123125818447E-17, -1.577721810442025713E-30, 1.000000000000000000 ) ) ;
#11490 = CARTESIAN_POINT ( 'NONE',  ( 7.000000000000006217, -5.999999999999981348, 6.250000000000005329 ) ) ;
#11491 = ORIENTED_EDGE ( 'NONE', *, *, #6824, .T. ) ;
#11492 = VECTOR ( 'NONE', #21628, 1000.000000000000114 ) ;
#11493 = CARTESIAN_POINT ( 'NONE',  ( -2.000000000000015543, -3.464101615137743728, 0.000000000000000000 ) ) ;
#11494 = LINE ( 'NONE', #13162, #17897 ) ;
#11495 = DIRECTION ( 'NONE',  ( -0.7071067811865456854, -0.7071067811865494601, -1.010793663541192964E-16 ) ) ;
#11496 = AXIS2_PLACEMENT_3D ( 'NONE', #18337, #6101, #5873 ) ;
#11497 = FACE_OUTER_BOUND ( 'NONE', #7226, .T. ) ;
#11498 = DIRECTION ( 'NONE',  ( 0.000000000000000000, 6.802837160693368935E-15, 1.000000000000000000 ) ) ;
#11499 = ORIENTED_EDGE ( 'NONE', *, *, #23048, .F. ) ;
#11500 = DIRECTION ( 'NONE',  ( 0.000000000000000000, 0.000000000000000000, 1.000000000000000000 ) ) ;
#11501 = DIRECTION ( 'NONE',  ( 0.000000000000000000, 0.000000000000000000, 1.000000000000000000 ) ) ;
#11502 = TOROIDAL_SURFACE ( 'NONE', #7031, 4.500000000000000888, 0.5000000000000000000 ) ;
#11503 = DIRECTION ( 'NONE',  ( 0.000000000000000000, 0.000000000000000000, -1.000000000000000000 ) ) ;
#11504 = CYLINDRICAL_SURFACE ( 'NONE', #8543, 2.100000000000011635 ) ;
#11505 = CARTESIAN_POINT ( 'NONE',  ( 3.950241966887847234, 3.393956070637395239, -1.121495646998965645 ) ) ;
#11506 = CARTESIAN_POINT ( 'NONE',  ( -3.999999999708153453, 35.49999999900384751, -25.50000000000000000 ) ) ;
#11507 = ADVANCED_FACE ( 'NONE', ( #16851 ), #20641, .F. ) ;
#11508 = CARTESIAN_POINT ( 'NONE',  ( -8.660254037844406838, 0.000000000000000000, 6.938893903907228378E-15 ) ) ;
#11509 = ORIENTED_EDGE ( 'NONE', *, *, #15166, .F. ) ;
#11510 = EDGE_CURVE ( 'NONE', #22149, #21928, #870, .T. ) ;
#11511 = AXIS2_PLACEMENT_3D ( 'NONE', #11440, #18507, #2734 ) ;
#11512 = CONTEXT_DEPENDENT_SHAPE_REPRESENTATION ( #7006, #4582 ) ;
#11513 = ORIENTED_EDGE ( 'NONE', *, *, #20306, .F. ) ;
#11514 = CIRCLE ( 'NONE', #11904, 2.000000000000015543 ) ;
#11515 = AXIS2_PLACEMENT_3D ( 'NONE', #14006, #14124, #24 ) ;
#11518 = EDGE_LOOP ( 'NONE', ( #20391, #952, #3690, #7316, #11662, #20680, #14741, #975 ) ) ;
#11517 = ADVANCED_FACE ( 'NONE', ( #6515 ), #9074, .F. ) ;
#11516 = VERTEX_POINT ( 'NONE', #20403 ) ;
#11519 = ADVANCED_FACE ( 'NONE', ( #7813 ), #15128, .T. ) ;
#11520 = AXIS2_PLACEMENT_3D ( 'NONE', #7114, #5456, #3570 ) ;
#11521 = DIRECTION ( 'NONE',  ( -2.013525853228507892E-32, -6.902532920683810383E-31, 1.000000000000000000 ) ) ;
#11522 = DIRECTION ( 'NONE',  ( -2.013525853228507892E-32, -6.902532920683810383E-31, 1.000000000000000000 ) ) ;
#11523 = ORIENTED_EDGE ( 'NONE', *, *, #4401, .F. ) ;
#11524 = CARTESIAN_POINT ( 'NONE',  ( 2.775557561562891351E-14, 10.49999999999998579, -3.000000000000002665 ) ) ;
#11525 = DIRECTION ( 'NONE',  ( -0.000000000000000000, 1.000000000000000000, -0.000000000000000000 ) ) ;
#11526 = CARTESIAN_POINT ( 'NONE',  ( 37.86602540378461157, 0.000000000000000000, -10.86602540378449255 ) ) ;
#11527 = CARTESIAN_POINT ( 'NONE',  ( -4.030227849471724078, 38.50929569396286212, -15.99955801060398031 ) ) ;
#11528 = CARTESIAN_POINT ( 'NONE',  ( -4.211140560182312420, 2.431303136016568889, -3.745885042887433958 ) ) ;
#11529 = TOROIDAL_SURFACE ( 'NONE', #10800, 6.000000000000000888, 3.000000000000000000 ) ;
#11530 = CARTESIAN_POINT ( 'NONE',  ( 54.42435809754118736, 0.4999999999999449329, -6.499999999999922728 ) ) ;
#11531 = CARTESIAN_POINT ( 'NONE',  ( 77.42435809754135789, -10.99999999999981526, 6.500000000000123457 ) ) ;
#11532 = EDGE_CURVE ( 'NONE', #3062, #17822, #20027, .T. ) ;
#11533 = EDGE_CURVE ( 'NONE', #13010, #688, #8757, .T. ) ;
#11534 = EDGE_CURVE ( 'NONE', #7463, #18297, #14746, .T. ) ;
#11535 = COLOUR_RGB ( '', 0.31764706, 0.68627451, 0.89019608) ;
#11536 = PLANE ( 'NONE',  #15562 ) ;
#11537 = DIRECTION ( 'NONE',  ( 0.000000000000000000, 0.000000000000000000, 1.000000000000000000 ) ) ;
#11538 = DIRECTION ( 'NONE',  ( -2.655250634480531216E-32, 6.902532920683810383E-31, -1.000000000000000000 ) ) ;
#11539 = DIRECTION ( 'NONE',  ( 0.000000000000000000, 0.000000000000000000, 1.000000000000000000 ) ) ;
#11540 = ORIENTED_EDGE ( 'NONE', *, *, #21013, .T. ) ;
#11541 = AXIS2_PLACEMENT_3D ( 'NONE', #2515, #5742, #9702 ) ;
#11542 = FILL_AREA_STYLE_COLOUR ( '', #10884 ) ;
#11544 = ORIENTED_EDGE ( 'NONE', *, *, #9964, .F. ) ;
#11543 = VERTEX_POINT ( 'NONE', #15082 ) ;
#11545 = EDGE_CURVE ( 'NONE', #13819, #6724, #9508, .T. ) ;
#11546 = AXIS2_PLACEMENT_3D ( 'NONE', #2168, #8404, #11568 ) ;
#11547 = ORIENTED_EDGE ( 'NONE', *, *, #3490, .T. ) ;
#11550 = ORIENTED_EDGE ( 'NONE', *, *, #19659, .F. ) ;
#11549 = EDGE_CURVE ( 'NONE', #8927, #13556, #7631, .T. ) ;
#11548 = ORIENTED_EDGE ( 'NONE', *, *, #9869, .F. ) ;
#11551 = CIRCLE ( 'NONE', #8560, 10.00000000000006395 ) ;
#11552 = ORIENTED_EDGE ( 'NONE', *, *, #18193, .F. ) ;
#11553 = CARTESIAN_POINT ( 'NONE',  ( 0.000000000000000000, 3.031088913245536087, 1.750000000000003331 ) ) ;
#11554 = ADVANCED_FACE ( 'NONE', ( #11565 ), #18749, .T. ) ;
#11555 = AXIS2_PLACEMENT_3D ( 'NONE', #9091, #16367, #20268 ) ;
#11556 = DIRECTION ( 'NONE',  ( -1.000000000000000000, 1.369518533665891191E-16, 3.560748187531317046E-15 ) ) ;
#11557 = VERTEX_POINT ( 'NONE', #19436 ) ;
#11558 = CARTESIAN_POINT ( 'NONE',  ( 37.00000000000014211, 10.49999999999999822, -3.000000000000002665 ) ) ;
#11559 = CARTESIAN_POINT ( 'NONE',  ( 4.024499207728609029, 2.323545700935586655, -3.572172305156459338 ) ) ;
#11560 = CYLINDRICAL_SURFACE ( 'NONE', #13273, 2.550000000000010481 ) ;
#11561 = CIRCLE ( 'NONE', #21343, 2.549999999999997158 ) ;
#11562 = CARTESIAN_POINT ( 'NONE',  ( 3.000000000291852764, 42.99999999900385461, -19.00000000000000355 ) ) ;
#11563 = CARTESIAN_POINT ( 'NONE',  ( -6.999999991915156095, -2.825498329575475420, 8.700799235122101294 ) ) ;
#11564 = AXIS2_PLACEMENT_3D ( 'NONE', #6487, #13668, #20855 ) ;
#11565 = FACE_OUTER_BOUND ( 'NONE', #15309, .T. ) ;
#11566 = CARTESIAN_POINT ( 'NONE',  ( 7.500000000000005329, -3.018576030000263533, 8.916666666666683838 ) ) ;
#11567 = PRESENTATION_STYLE_ASSIGNMENT (( #16855 ) ) ;
#11568 = DIRECTION ( 'NONE',  ( -1.000000000000000000, 0.000000000000000000, 0.000000000000000000 ) ) ;
#11569 = CARTESIAN_POINT ( 'NONE',  ( 10.49999999999999467, -13.50000000000000888, 9.250000000000063949 ) ) ;
#11570 = CARTESIAN_POINT ( 'NONE',  ( -6.899936419963479395, 13.99939863585067990, -26.79405629275723655 ) ) ;
#11571 = CARTESIAN_POINT ( 'NONE',  ( 4.033895293471146282, 1.419609371826101141, -3.500000000000006217 ) ) ;
#11572 = AXIS2_PLACEMENT_3D ( 'NONE', #23200, #10137, #12001 ) ;
#11573 = ORIENTED_EDGE ( 'NONE', *, *, #22746, .F. ) ;
#11575 = ORIENTED_EDGE ( 'NONE', *, *, #10968, .F. ) ;
#11574 = VERTEX_POINT ( 'NONE', #14035 ) ;
#11576 = AXIS2_PLACEMENT_3D ( 'NONE', #6453, #8454, #21042 ) ;
#11577 = EDGE_CURVE ( 'NONE', #14890, #16829, #7276, .T. ) ;
#11578 = VERTEX_POINT ( 'NONE', #10267 ) ;
#11579 = AXIS2_PLACEMENT_3D ( 'NONE', #7391, #15964, #9038 ) ;
#11580 = ORIENTED_EDGE ( 'NONE', *, *, #19442, .T. ) ;
#11581 = CONICAL_SURFACE ( 'NONE', #8582, 7.500000000000001776, 1.308996938995750092 ) ;
#11582 = EDGE_CURVE ( 'NONE', #3321, #23117, #20418, .T. ) ;
#11583 = VERTEX_POINT ( 'NONE', #1341 ) ;
#11584 = CARTESIAN_POINT ( 'NONE',  ( 5.600000000000000533, 2.020725942163612121, 3.499999999999957812 ) ) ;
#11585 = B_SPLINE_CURVE_WITH_KNOTS ( 'NONE', 3,
 ( #5734, #21734, #9376, #3722, #5620, #12901, #4176, #16523 ),
 .UNSPECIFIED., .F., .F.,
 ( 4, 2, 2, 4 ),
 ( 2.465131517636197337E-07, 0.001183067374689898569, 0.001774477805458966450, 0.002365888236228034115 ),
 .UNSPECIFIED. ) ;
#11586 = CARTESIAN_POINT ( 'NONE',  ( 2.499999999999998668, 2.000000000000001776, -19.00000000000001066 ) ) ;
#11587 = EDGE_LOOP ( 'NONE', ( #3920, #20508, #20622, #9249 ) ) ;
#11588 =( GEOMETRIC_REPRESENTATION_CONTEXT ( 3 ) GLOBAL_UNCERTAINTY_ASSIGNED_CONTEXT ( ( #11687 ) ) GLOBAL_UNIT_ASSIGNED_CONTEXT ( ( #14760, #4054, #2290 ) ) REPRESENTATION_CONTEXT ( 'NONE', 'WORKASPACE' ) );
#11589 = CARTESIAN_POINT ( 'NONE',  ( -12.84999999999999964, -2.000000000000001776, 0.000000000000000000 ) ) ;
#11590 = CARTESIAN_POINT ( 'NONE',  ( 4.082498951862915781, 2.020725942163681399, 3.499999999999996003 ) ) ;
#11591 = CARTESIAN_POINT ( 'NONE',  ( 6.827186199083545087E-16, -11.33467790002633002, -7.208584908080457154 ) ) ;
#11592 = DIRECTION ( 'NONE',  ( -1.000000000000000000, 0.000000000000000000, -1.066879592304109953E-26 ) ) ;
#11593 = CARTESIAN_POINT ( 'NONE',  ( -7.710998176012597405, -11.54387914083317668, 8.114728912742389610 ) ) ;
#11594 = CARTESIAN_POINT ( 'NONE',  ( -8.115139842999290920, -13.89206392873134099, 7.423524081915784834 ) ) ;
#11595 = TOROIDAL_SURFACE ( 'NONE', #21016, 5.500000000000000000, 0.5000000000000000000 ) ;
#11596 = CARTESIAN_POINT ( 'NONE',  ( 1.446367150925043532, 4.999999999999985789, -7.500000000000003553 ) ) ;
#11597 = CARTESIAN_POINT ( 'NONE',  ( 30.00000000029184832, -9.961476088449217059E-10, -5.999999999999998224 ) ) ;
#11598 = CARTESIAN_POINT ( 'NONE',  ( 37.22062532321636752, 0.1155932590976526397, -10.54332536350026750 ) ) ;
#11599 = ORIENTED_EDGE ( 'NONE', *, *, #15551, .T. ) ;
#11600 = FILL_AREA_STYLE_COLOUR ( '', #22502 ) ;
#11601 = CARTESIAN_POINT ( 'NONE',  ( 4.050880675075977599, -1.379097446046351649, -3.567934390854435645 ) ) ;
#11602 = CARTESIAN_POINT ( 'NONE',  ( 55.36587326203805048, 4.009651402420072230, -5.999999999999963585 ) ) ;
#11603 = ORIENTED_EDGE ( 'NONE', *, *, #22762, .T. ) ;
#11604 = STYLED_ITEM ( 'NONE', ( #8171 ), #6953 ) ;
#11605 = EDGE_LOOP ( 'NONE', ( #15362, #2000, #10544, #7828 ) ) ;
#11606 = ORIENTED_EDGE ( 'NONE', *, *, #17181, .T. ) ;
#11607 = ORIENTED_EDGE ( 'NONE', *, *, #7124, .F. ) ;
#11608 = DIRECTION ( 'NONE',  ( -1.066788928082016908E-26, -3.471809175856251779E-58, 1.000000000000000000 ) ) ;
#11609 = TOROIDAL_SURFACE ( 'NONE', #21415, 4.500000000000000888, 0.5000000000000000000 ) ;
#11610 = CARTESIAN_POINT ( 'NONE',  ( -10.50000000000000888, 0.000000000000000000, 9.249999999999994671 ) ) ;
#11611 = ORIENTED_EDGE ( 'NONE', *, *, #2195, .T. ) ;
#11612 = AXIS2_PLACEMENT_3D ( 'NONE', #11351, #20085, #5735 ) ;
#11613 = DIRECTION ( 'NONE',  ( -0.7071067811865530128, 8.659560562354856437E-17, -0.7071067811865421326 ) ) ;
#11614 = CARTESIAN_POINT ( 'NONE',  ( 108.9540049198142100, -11.33354449810611264, 6.000000000000088818 ) ) ;
#11615 = DIRECTION ( 'NONE',  ( -1.000000000000000000, 1.847414967615758933E-47, -3.885780586188017323E-16 ) ) ;
#11616 = CARTESIAN_POINT ( 'NONE',  ( -4.550510256924972907, 36.49999999900384751, -19.00000000000000355 ) ) ;
#11617 = DIRECTION ( 'NONE',  ( 1.000000000000000000, 0.000000000000000000, 0.000000000000000000 ) ) ;
#11618 = VECTOR ( 'NONE', #15518, 1000.000000000000114 ) ;
#11619 = CARTESIAN_POINT ( 'NONE',  ( 10.49999999999999467, -2.000000000000001776, 9.249999999999980460 ) ) ;
#11620 = FACE_OUTER_BOUND ( 'NONE', #3431, .T. ) ;
#11621 = PRODUCT_DEFINITION_FORMATION_WITH_SPECIFIED_SOURCE ( 'ANY', '', #18870, .NOT_KNOWN. ) ;
#11622 = EDGE_CURVE ( 'NONE', #10141, #16719, #22296, .T. ) ;
#11623 = CARTESIAN_POINT ( 'NONE',  ( -6.938893903907228378E-14, -4.618802153517020059, -0.3572655899081733644 ) ) ;
#11624 = CARTESIAN_POINT ( 'NONE',  ( 0.000000000000000000, 0.000000000000000000, 0.000000000000000000 ) ) ;
#11625 = CARTESIAN_POINT ( 'NONE',  ( 1.558781775088847367E-15, -2.686816014504586736, -2.346298152288353034 ) ) ;
#11626 = DIRECTION ( 'NONE',  ( -5.598259082250079541E-17, 1.000000000000000000, -6.162975822039171151E-32 ) ) ;
#11627 = CARTESIAN_POINT ( 'NONE',  ( 6.938893903907228378E-15, 4.618802153517023612, -3.433295621305385126 ) ) ;
#11628 = CARTESIAN_POINT ( 'NONE',  ( 77.42435809754140053, -6.999999999999811706, -5.999999999999984901 ) ) ;
#11629 = ORIENTED_EDGE ( 'NONE', *, *, #4829, .F. ) ;
#11630 = ITEM_DEFINED_TRANSFORMATION ( 'NONE', 'NONE', #15382,  #22115 ) ;
#11631 = AXIS2_PLACEMENT_3D ( 'NONE', #8763, #3468, #19581 ) ;
#11632 = ORIENTED_EDGE ( 'NONE', *, *, #16277, .F. ) ;
#11634 = ORIENTED_EDGE ( 'NONE', *, *, #9360, .T. ) ;
#11633 = ORIENTED_EDGE ( 'NONE', *, *, #1458, .T. ) ;
#11635 = CARTESIAN_POINT ( 'NONE',  ( 8.697224362268011433, -12.50000000000002842, 6.250000000000061284 ) ) ;
#11636 = DIRECTION ( 'NONE',  ( -1.000000000000000000, -3.254448077276381206E-32, 1.066786462891689527E-26 ) ) ;
#11637 = ADVANCED_FACE ( 'NONE', ( #21341, #3224, #17438 ), #8506, .F. ) ;
#11638 = CARTESIAN_POINT ( 'NONE',  ( 2.499999999999992006, 2.000000000000001776, -0.2500000000000349165 ) ) ;
#11639 = ORIENTED_EDGE ( 'NONE', *, *, #1347, .F. ) ;
#11640 = CARTESIAN_POINT ( 'NONE',  ( 4.071447262713891568, 4.041451884327377009, -2.081668171172168513E-14 ) ) ;
#11641 = DIRECTION ( 'NONE',  ( 3.885780586188016830E-16, 4.437342591868156373E-31, -1.000000000000000000 ) ) ;
#11642 = DIRECTION ( 'NONE',  ( 2.220446049250313081E-16, -1.000000000000000000, 7.025792437124636392E-31 ) ) ;
#11643 = ADVANCED_FACE ( 'NONE', ( #10380 ), #15558, .F. ) ;
#11644 = DIRECTION ( 'NONE',  ( -1.000000000000000000, -4.440892098500626162E-16, 5.551115123125782702E-16 ) ) ;
#11645 = DIRECTION ( 'NONE',  ( 0.6819983600624998088, 0.7313537016191693496, 0.000000000000000000 ) ) ;
#11646 = CIRCLE ( 'NONE', #6040, 5.371010071662839280 ) ;
#11647 = CARTESIAN_POINT ( 'NONE',  ( -3.673643420401913939, -2.497823135841291009, -5.351519936624987928 ) ) ;
#11648 = FACE_OUTER_BOUND ( 'NONE', #10088, .T. ) ;
#11649 = DIRECTION ( 'NONE',  ( 0.000000000000000000, -1.000000000000000000, 0.000000000000000000 ) ) ;
#11650 = SHAPE_REPRESENTATION ( 'Rod', ( #22115 ), #19511 ) ;
#11651 = EDGE_CURVE ( 'NONE', #21020, #7712, #14029, .T. ) ;
#11652 = DIRECTION ( 'NONE',  ( -0.000000000000000000, -0.000000000000000000, 1.000000000000000000 ) ) ;
#11653 = ADVANCED_FACE ( 'NONE', ( #23222 ), #18528, .F. ) ;
#11654 = DIRECTION ( 'NONE',  ( -4.190823558986625216E-31, 1.000000000000000000, -4.190823558986625216E-31 ) ) ;
#11655 = LINE ( 'NONE', #9908, #7780 ) ;
#11656 = ADVANCED_FACE ( 'NONE', ( #8737 ), #12019, .F. ) ;
#11657 = ORIENTED_EDGE ( 'NONE', *, *, #10549, .T. ) ;
#11659 = ORIENTED_EDGE ( 'NONE', *, *, #7168, .T. ) ;
#11658 = ORIENTED_EDGE ( 'NONE', *, *, #1904, .T. ) ;
#11660 = ORIENTED_EDGE ( 'NONE', *, *, #6032, .T. ) ;
#11662 = ORIENTED_EDGE ( 'NONE', *, *, #7180, .T. ) ;
#11661 = ORIENTED_EDGE ( 'NONE', *, *, #17685, .F. ) ;
#11663 = CIRCLE ( 'NONE', #12425, 2.549999999999997158 ) ;
#11664 = CARTESIAN_POINT ( 'NONE',  ( 4.175813232069142344, 2.061359961916322980, 3.570380186727409200 ) ) ;
#11665 = CARTESIAN_POINT ( 'NONE',  ( -64.00000000000038369, -3.200000000000088107, -2.000000000000029310 ) ) ;
#11666 = VERTEX_POINT ( 'NONE', #6991 ) ;
#11667 = EDGE_CURVE ( 'NONE', #19930, #21802, #15512, .T. ) ;
#11668 = FILL_AREA_STYLE_COLOUR ( '', #7279 ) ;
#11669 = ADVANCED_FACE ( 'NONE', ( #19206 ), #8019, .T. ) ;
#11670 = CARTESIAN_POINT ( 'NONE',  ( 24.75000000000000355, 2.000000000000029310, -1.500000000000004885 ) ) ;
#11671 = DIRECTION ( 'NONE',  ( 0.000000000000000000, 0.000000000000000000, 1.000000000000000000 ) ) ;
#11672 = CARTESIAN_POINT ( 'NONE',  ( 4.000000000000003553, 2.309401076758525573, -0.3572655899081733644 ) ) ;
#11673 = DIRECTION ( 'NONE',  ( 0.000000000000000000, 0.000000000000000000, -1.000000000000000000 ) ) ;
#11674 = CARTESIAN_POINT ( 'NONE',  ( 3.999999999999975131, -2.511475576507315566, -3.469253905236648006 ) ) ;
#11675 = DIRECTION ( 'NONE',  ( -1.000000000000000000, -3.254448077276381206E-32, -1.066788928082016908E-26 ) ) ;
#11676 = DIRECTION ( 'NONE',  ( 1.000000000000000000, 1.910522504832140594E-31, -5.551115123125818447E-17 ) ) ;
#11677 = CARTESIAN_POINT ( 'NONE',  ( 37.43301270189239460, 0.2500000000000002220, -2.999999999999988898 ) ) ;
#11678 = LINE ( 'NONE', #13803, #6672 ) ;
#11679 = EDGE_CURVE ( 'NONE', #3004, #17067, #8778, .T. ) ;
#11680 = CARTESIAN_POINT ( 'NONE',  ( 108.2426266706970779, -6.527605602963587828, 6.000000000000109246 ) ) ;
#11681 = CIRCLE ( 'NONE', #21485, 4.000000000000023093 ) ;
#11682 =( GEOMETRIC_REPRESENTATION_CONTEXT ( 3 ) GLOBAL_UNCERTAINTY_ASSIGNED_CONTEXT ( ( #15192 ) ) GLOBAL_UNIT_ASSIGNED_CONTEXT ( ( #3135, #5363, #10418 ) ) REPRESENTATION_CONTEXT ( 'NONE', 'WORKASPACE' ) );
#11683 = CARTESIAN_POINT ( 'NONE',  ( 80.15235153779138955, -8.074585193523137860, 6.500000000000040856 ) ) ;
#11684 = DIRECTION ( 'NONE',  ( 0.000000000000000000, 3.469446951953618922E-15, 1.000000000000000000 ) ) ;
#11685 = EDGE_CURVE ( 'NONE', #3914, #20222, #14384, .T. ) ;
#11686 = EDGE_LOOP ( 'NONE', ( #21607, #11215, #2442, #16568 ) ) ;
#11687 = UNCERTAINTY_MEASURE_WITH_UNIT (LENGTH_MEASURE( 1.000000000000000082E-05 ), #14760, 'distance_accuracy_value', 'NONE');
#11689 = VERTEX_POINT ( 'NONE', #19683 ) ;
#11688 = ORIENTED_EDGE ( 'NONE', *, *, #18000, .F. ) ;
#11690 = EDGE_CURVE ( 'NONE', #18297, #1148, #12142, .T. ) ;
#11691 = VERTEX_POINT ( 'NONE', #1446 ) ;
#11692 = ORIENTED_EDGE ( 'NONE', *, *, #1501, .T. ) ;
#11693 = EDGE_LOOP ( 'NONE', ( #14970, #3260, #22708, #628 ) ) ;
#11694 = ORIENTED_EDGE ( 'NONE', *, *, #21348, .T. ) ;
#11695 = CARTESIAN_POINT ( 'NONE',  ( 4.175075985190096262, -2.060370777630091244, 3.568666869285578969 ) ) ;
#11696 = EDGE_CURVE ( 'NONE', #14335, #18914, #14401, .T. ) ;
#11697 = CIRCLE ( 'NONE', #21856, 7.000000000000006217 ) ;
#11698 = CIRCLE ( 'NONE', #21857, 0.5000000000000004441 ) ;
#11699 = CARTESIAN_POINT ( 'NONE',  ( -12.84999999999999964, 0.000000000000000000, 0.000000000000000000 ) ) ;
#11700 = ORIENTED_EDGE ( 'NONE', *, *, #6745, .F. ) ;
#11701 = ORIENTED_EDGE ( 'NONE', *, *, #7533, .F. ) ;
#11702 = CARTESIAN_POINT ( 'NONE',  ( 6.500000000000283329, 1.942890293094023946E-13, -5.999999999999943157 ) ) ;
#11703 = DIRECTION ( 'NONE',  ( -1.000000000000000000, 1.577021341797087946E-16, -5.322447028565171744E-15 ) ) ;
#11704 = DIRECTION ( 'NONE',  ( -1.000000000000000000, 0.000000000000000000, 0.000000000000000000 ) ) ;
#11705 = DIRECTION ( 'NONE',  ( -0.000000000000000000, -0.000000000000000000, -1.000000000000000000 ) ) ;
#11706 = EDGE_CURVE ( 'NONE', #5239, #13382, #21175, .T. ) ;
#11707 = CARTESIAN_POINT ( 'NONE',  ( -7.000000000000033751, -10.98142396999974579, 8.916666666666724694 ) ) ;
#11708 = DIRECTION ( 'NONE',  ( -7.860214984770699307E-18, 1.409037165336591006E-16, 1.000000000000000000 ) ) ;
#11709 = FACE_OUTER_BOUND ( 'NONE', #12976, .T. ) ;
#11710 = CARTESIAN_POINT ( 'NONE',  ( 1.387778780781445676E-14, 4.163336342344337027E-14, -2.000000000000001776 ) ) ;
#11711 = CARTESIAN_POINT ( 'NONE',  ( 109.3164911904586774, -11.67918431276168612, -6.500000000000054179 ) ) ;
#11712 = ORIENTED_EDGE ( 'NONE', *, *, #9301, .T. ) ;
#11713 = DIRECTION ( 'NONE',  ( -1.733449886265891589E-32, 4.190823558986610327E-31, -1.000000000000000000 ) ) ;
#11715 = AXIS2_PLACEMENT_3D ( 'NONE', #22249, #4476, #20497 ) ;
#11714 = DIRECTION ( 'NONE',  ( -1.000000000000000000, 0.000000000000000000, 0.000000000000000000 ) ) ;
#11716 = VECTOR ( 'NONE', #9752, 1000.000000000000000 ) ;
#11717 = B_SPLINE_CURVE_WITH_KNOTS ( 'NONE', 3,
 ( #13946, #12178, #19363, #1489, #3262, #5130 ),
 .UNSPECIFIED., .F., .F.,
 ( 4, 2, 4 ),
 ( 0.000000000000000000, 0.002086519881787260184, 0.004173039763574519501 ),
 .UNSPECIFIED. ) ;
#11718 = ORIENTED_EDGE ( 'NONE', *, *, #12246, .T. ) ;
#11719 = CIRCLE ( 'NONE', #19246, 0.5000000000000000000 ) ;
#11720 = ORIENTED_EDGE ( 'NONE', *, *, #22317, .F. ) ;
#11721 = VERTEX_POINT ( 'NONE', #21797 ) ;
#11722 = PRODUCT_DEFINITION_SHAPE ( 'NONE', 'NONE',  #23284 ) ;
#11723 = ORIENTED_EDGE ( 'NONE', *, *, #8805, .T. ) ;
#11724 = CARTESIAN_POINT ( 'NONE',  ( 2.775557561562891351E-14, 0.000000000000000000, -3.000000000000002665 ) ) ;
#11725 = CARTESIAN_POINT ( 'NONE',  ( -4.499999999708154341, 35.49999999900384751, -19.50000000000000355 ) ) ;
#11726 = VERTEX_POINT ( 'NONE', #19795 ) ;
#11727 = AXIS2_PLACEMENT_3D ( 'NONE', #13113, #22282, #650 ) ;
#11728 = DIRECTION ( 'NONE',  ( -1.000000000000000000, 0.000000000000000000, 0.000000000000000000 ) ) ;
#11729 = DIRECTION ( 'NONE',  ( -1.000000000000000000, 1.550910762415566494E-16, -8.566929763922626680E-48 ) ) ;
#11730 = CARTESIAN_POINT ( 'NONE',  ( 0.000000000000000000, 0.000000000000000000, 0.000000000000000000 ) ) ;
#11731 = VERTEX_POINT ( 'NONE', #4010 ) ;
#11732 = DIRECTION ( 'NONE',  ( 3.885780586188016830E-16, 4.437342591868156373E-31, -1.000000000000000000 ) ) ;
#11733 = CARTESIAN_POINT ( 'NONE',  ( 4.055492966679525857, 2.385006769472625354, 3.005124364834308892 ) ) ;
#11734 = CARTESIAN_POINT ( 'NONE',  ( 4.182608627552025560, 0.7500000000000556222, -2.876096987965587104 ) ) ;
#11735 = CIRCLE ( 'NONE', #2347, 2.500000000000002220 ) ;
#11736 = EDGE_CURVE ( 'NONE', #7321, #919, #17777, .T. ) ;
#11737 = AXIS2_PLACEMENT_3D ( 'NONE', #21274, #1841, #5392 ) ;
#11738 = DIRECTION ( 'NONE',  ( -1.550910762415566494E-16, -1.000000000000000000, 8.135128085091684243E-31 ) ) ;
#11739 = AXIS2_PLACEMENT_3D ( 'NONE', #18736, #22153, #2388 ) ;
#11740 = CARTESIAN_POINT ( 'NONE',  ( 35.50000000029185543, 16.99999999900385461, -26.00000000000000000 ) ) ;
#11741 = CARTESIAN_POINT ( 'NONE',  ( 37.00000000000014211, 0.000000000000000000, -9.999999999999980460 ) ) ;
#11742 = DIRECTION ( 'NONE',  ( -6.656013887802287108E-31, -1.000000000000000000, 3.469446951953609061E-15 ) ) ;
#11743 = LINE ( 'NONE', #2818, #272 ) ;
#11744 = CARTESIAN_POINT ( 'NONE',  ( -3.333333333333423631, 2.694301256218305518, -3.300726591567079371 ) ) ;
#11745 = EDGE_CURVE ( 'NONE', #16893, #19599, #20047, .T. ) ;
#11746 = CARTESIAN_POINT ( 'NONE',  ( 2.918498775983380256E-10, 2.999999999003851503, -26.00000000000000000 ) ) ;
#11747 =( BOUNDED_SURFACE ( )  B_SPLINE_SURFACE ( 3, 2, ( 
 ( #104, #14550, #21407 ),
 ( #7281, #19506, #17980 ),
 ( #8804, #19745, #12435 ),
 ( #3837, #14323, #5399 ),
 ( #12786, #3401, #7047 ),
 ( #14448, #10560, #3510 ),
 ( #3622, #1624, #1734 ),
 ( #19967, #17620, #10789 ) ),
 .UNSPECIFIED., .F., .F., .F. ) 
 B_SPLINE_SURFACE_WITH_KNOTS ( ( 4, 2, 2, 4 ),
 ( 3, 3 ),
 ( 3.665191429188094485, 3.926990816987243171, 4.188790204786392302, 4.712388980384689674 ),
 ( 0.000000000000000000, 1.000000000000000000 ),
 .UNSPECIFIED. ) 
 GEOMETRIC_REPRESENTATION_ITEM ( )  RATIONAL_B_SPLINE_SURFACE ( (
 ( 1.000000000000000000, 0.7905694150421800348, 1.000000000000000000),
 ( 1.000000000000000000, 0.8144940154005646527, 1.000000000000000000),
 ( 1.000000000000000000, 0.8408337562111951602, 1.000000000000000000),
 ( 1.000000000000000000, 0.8912170513578159259, 1.000000000000000000),
 ( 1.000000000000000000, 0.9152160911082961592, 1.000000000000000000),
 ( 1.000000000000000000, 0.9758108578640052322, 1.000000000000000000),
 ( 1.000000000000000000, 1.000509427570091203, 1.000000000000000000),
 ( 1.000000000000000000, 1.000000000000000000, 1.000000000000000000) ) ) 
 REPRESENTATION_ITEM ( '' )  SURFACE ( )  );
#11748 = CONTEXT_DEPENDENT_SHAPE_REPRESENTATION ( #2941, #7970 ) ;
#11749 = CIRCLE ( 'NONE', #17773, 0.2500000000000002220 ) ;
#11750 = EDGE_LOOP ( 'NONE', ( #19467, #12087, #22707, #5489 ) ) ;
#11751 = B_SPLINE_CURVE_WITH_KNOTS ( 'NONE', 3,
 ( #17378, #15266, #11625, #15503 ),
 .UNSPECIFIED., .F., .F.,
 ( 4, 4 ),
 ( 2.380739282734603470E-07, 0.002044882221487528875 ),
 .UNSPECIFIED. ) ;
#11752 = CIRCLE ( 'NONE', #7630, 4.749999999999986677 ) ;
#11753 = TOROIDAL_SURFACE ( 'NONE', #2348, 3.299999999999999822, 0.5000000000000000000 ) ;
#11754 = AXIS2_PLACEMENT_3D ( 'NONE', #7764, #11406, #21788 ) ;
#11756 = ORIENTED_EDGE ( 'NONE', *, *, #3043, .F. ) ;
#11755 = VERTEX_POINT ( 'NONE', #161 ) ;
#11757 = CARTESIAN_POINT ( 'NONE',  ( 124.5000000000018332, -4.000000000000058620, -5.999999999999943157 ) ) ;
#11758 = CYLINDRICAL_SURFACE ( 'NONE', #9227, 0.5000000000000004441 ) ;
#11759 = DIRECTION ( 'NONE',  ( 1.000000000000000000, 0.000000000000000000, 0.000000000000000000 ) ) ;
#11760 = ORIENTED_EDGE ( 'NONE', *, *, #10869, .T. ) ;
#11761 = DIRECTION ( 'NONE',  ( 0.000000000000000000, 1.000000000000000000, 0.000000000000000000 ) ) ;
#11762 = CARTESIAN_POINT ( 'NONE',  ( -6.999999999999992006, -1.390227771353544473, 9.249999999999994671 ) ) ;
#11763 = DIRECTION ( 'NONE',  ( -0.7453559924999295649, 0.000000000000000000, 0.6666666666666669627 ) ) ;
#11764 = CARTESIAN_POINT ( 'NONE',  ( -95.20000000000065654, -9.714451465470119729E-14, -2.000000000000001776 ) ) ;
#11765 = DIRECTION ( 'NONE',  ( 2.013525853228507892E-32, 6.902532920683810383E-31, -1.000000000000000000 ) ) ;
#11766 = VECTOR ( 'NONE', #7990, 1000.000000000000000 ) ;
#11767 = CYLINDRICAL_SURFACE ( 'NONE', #821, 0.4999999999999978351 ) ;
#11768 = TOROIDAL_SURFACE ( 'NONE', #1634, 4.500000000000000888, 0.5000000000000000000 ) ;
#11769 = DIRECTION ( 'NONE',  ( -0.6819983600624981435, -0.7313537016191709039, 0.000000000000000000 ) ) ;
#11770 = AXIS2_PLACEMENT_3D ( 'NONE', #17639, #21428, #12695 ) ;
#11771 = CARTESIAN_POINT ( 'NONE',  ( -6.000000000000019540, -7.500000000000007105, 7.500000000000062172 ) ) ;
#11772 = AXIS2_PLACEMENT_3D ( 'NONE', #10336, #15744, #6816 ) ;
#11773 = DIRECTION ( 'NONE',  ( 1.000000000000000000, 0.000000000000000000, 0.000000000000000000 ) ) ;
#11774 = VECTOR ( 'NONE', #5524, 1000.000000000000000 ) ;
#11775 = DIRECTION ( 'NONE',  ( -1.550910762415566494E-16, -1.000000000000000000, 8.135128085091684243E-31 ) ) ;
#11776 = DIRECTION ( 'NONE',  ( 0.000000000000000000, -0.000000000000000000, 1.000000000000000000 ) ) ;
#11777 = ORIENTED_EDGE ( 'NONE', *, *, #20306, .T. ) ;
#11778 = PRODUCT_DEFINITION ( 'UNKNOWN', '', #19538, #14989 ) ;
#11779 = DIRECTION ( 'NONE',  ( 0.000000000000000000, 0.000000000000000000, 1.000000000000000000 ) ) ;
#11781 = EDGE_LOOP ( 'NONE', ( #21180, #21923, #19221, #3486, #21695, #5011 ) ) ;
#11780 = ORIENTED_EDGE ( 'NONE', *, *, #3796, .T. ) ;
#11782 = EDGE_CURVE ( 'NONE', #4634, #8517, #2129, .T. ) ;
#11783 = EDGE_LOOP ( 'NONE', ( #18268, #13303, #250, #17904 ) ) ;
#11784 = VECTOR ( 'NONE', #21018, 1000.000000000000114 ) ;
#11786 = ORIENTED_EDGE ( 'NONE', *, *, #3345, .F. ) ;
#11785 = ORIENTED_EDGE ( 'NONE', *, *, #14191, .F. ) ;
#11787 = ORIENTED_EDGE ( 'NONE', *, *, #16040, .T. ) ;
#11788 = DIRECTION ( 'NONE',  ( 3.885780586188016830E-16, 4.437342591868156373E-31, -1.000000000000000000 ) ) ;
#11789 = AXIS2_PLACEMENT_3D ( 'NONE', #11610, #9979, #4787 ) ;
#11790 = LINE ( 'NONE', #15432, #21600 ) ;
#11791 = LINE ( 'NONE', #18978, #1311 ) ;
#11792 = ADVANCED_FACE ( 'NONE', ( #10846 ), #3675, .T. ) ;
#11793 = LINE ( 'NONE', #18980, #8489 ) ;
#11794 =( REPRESENTATION_RELATIONSHIP ('NONE','NONE', #19450, #981 ) REPRESENTATION_RELATIONSHIP_WITH_TRANSFORMATION ( #22470 )SHAPE_REPRESENTATION_RELATIONSHIP( ) );
#11795 = CARTESIAN_POINT ( 'NONE',  ( 37.00000000000014211, 0.000000000000000000, -9.999999999999980460 ) ) ;
#11796 = DIRECTION ( 'NONE',  ( 9.693647360340828445E-26, 0.000000000000000000, -1.000000000000000000 ) ) ;
#11797 = CARTESIAN_POINT ( 'NONE',  ( 4.163336342344337027E-14, 3.469446951953614189E-14, -3.000000000000002665 ) ) ;
#11798 = CARTESIAN_POINT ( 'NONE',  ( -6.959810536856680940, 36.00015702695179698, -26.48940942388196618 ) ) ;
#11799 = DIRECTION ( 'NONE',  ( 0.000000000000000000, -1.431146867680864591E-14, -1.000000000000000000 ) ) ;
#11800 = CARTESIAN_POINT ( 'NONE',  ( 63.19496167919710672, -3.291091657286276728, 6.000000000000123457 ) ) ;
#11801 = EDGE_CURVE ( 'NONE', #22849, #8024, #3141, .T. ) ;
#11802 = CARTESIAN_POINT ( 'NONE',  ( 12.49999999999995914, 2.775557561562891036E-14, -14.25000000000000355 ) ) ;
#11803 = CARTESIAN_POINT ( 'NONE',  ( -4.000000000000003553, -2.309401076758532678, -0.3572655899081733644 ) ) ;
#11804 = AXIS2_PLACEMENT_3D ( 'NONE', #8157, #19327, #11905 ) ;
#11805 = CIRCLE ( 'NONE', #22716, 10.00000000000006395 ) ;
#11806 = CARTESIAN_POINT ( 'NONE',  ( -8.495599073428101278, -12.48424298295908130, 7.013360899078390887 ) ) ;
#11807 = CARTESIAN_POINT ( 'NONE',  ( 88.75737332930592061, -6.527605602963476805, -6.000000000000012434 ) ) ;
#11808 = DIRECTION ( 'NONE',  ( 1.000000000000000000, 1.421085471520213625E-14, 3.854941057726199147E-16 ) ) ;
#11809 = AXIS2_PLACEMENT_3D ( 'NONE', #2187, #18420, #7717 ) ;
#11810 = EDGE_LOOP ( 'NONE', ( #3555, #13851 ) ) ;
#11811 = EDGE_CURVE ( 'NONE', #4916, #16467, #3148, .T. ) ;
#11812 = SURFACE_STYLE_USAGE ( .BOTH. , #15095 ) ;
#11814 = ORIENTED_EDGE ( 'NONE', *, *, #19155, .T. ) ;
#11813 = ORIENTED_EDGE ( 'NONE', *, *, #1210, .F. ) ;
#11815 = EDGE_CURVE ( 'NONE', #11464, #19280, #16265, .T. ) ;
#11816 = ORIENTED_EDGE ( 'NONE', *, *, #16907, .T. ) ;
#11817 = ORIENTED_EDGE ( 'NONE', *, *, #1042, .F. ) ;
#11818 = ORIENTED_EDGE ( 'NONE', *, *, #15718, .T. ) ;
#11819 = ORIENTED_EDGE ( 'NONE', *, *, #22043, .T. ) ;
#11820 = DIRECTION ( 'NONE',  ( 2.172745813409348851E-17, -1.000000000000000000, -3.406761633869148826E-16 ) ) ;
#11821 = PRESENTATION_LAYER_ASSIGNMENT (  '', '', ( #4302 ) ) ;
#11822 = EDGE_CURVE ( 'NONE', #6879, #1883, #9081, .T. ) ;
#11823 = ADVANCED_FACE ( 'NONE', ( #46 ), #14715, .F. ) ;
#11824 = CARTESIAN_POINT ( 'NONE',  ( 36.00000000029184832, 5.999999999003851059, -28.99999999999999645 ) ) ;
#11825 = ORIENTED_EDGE ( 'NONE', *, *, #3345, .T. ) ;
#11826 = DIRECTION ( 'NONE',  ( 0.000000000000000000, 0.000000000000000000, 1.000000000000000000 ) ) ;
#11827 = FACE_OUTER_BOUND ( 'NONE', #22788, .T. ) ;
#11828 = LINE ( 'NONE', #15585, #4987 ) ;
#11829 = DIRECTION ( 'NONE',  ( 0.000000000000000000, 0.000000000000000000, -1.000000000000000000 ) ) ;
#11830 = CARTESIAN_POINT ( 'NONE',  ( 108.2426266706970637, -13.02760560296359316, 5.999999999999984901 ) ) ;
#11831 = CARTESIAN_POINT ( 'NONE',  ( 4.175813232069142344, 4.122719923832743660, 0.000000000000000000 ) ) ;
#11832 = CARTESIAN_POINT ( 'NONE',  ( -45.01801948466083303, -6.474873734152952309, 8.000000000000062172 ) ) ;
#11833 = CARTESIAN_POINT ( 'NONE',  ( -89.70000000000055707, -3.200000000000091660, -1.999999999999946265 ) ) ;
#11834 = DIRECTION ( 'NONE',  ( 1.550910762415566494E-16, 1.000000000000000000, -8.135128085091684243E-31 ) ) ;
#11835 = DIRECTION ( 'NONE',  ( 0.000000000000000000, 0.000000000000000000, 1.000000000000000000 ) ) ;
#11836 = EDGE_CURVE ( 'NONE', #4144, #1136, #6141, .T. ) ;
#11837 = ORIENTED_EDGE ( 'NONE', *, *, #9531, .F. ) ;
#11838 = ADVANCED_FACE ( 'NONE', ( #7330 ), #16360, .F. ) ;
#11839 = EDGE_CURVE ( 'NONE', #10566, #16898, #19276, .T. ) ;
#11840 = LINE ( 'NONE', #1265, #3336 ) ;
#11841 = VECTOR ( 'NONE', #14571, 1000.000000000000000 ) ;
#11842 = CARTESIAN_POINT ( 'NONE',  ( -3.999999999708153453, 13.99999999900385106, -22.50000000000000000 ) ) ;
#11843 = ORIENTED_EDGE ( 'NONE', *, *, #2823, .T. ) ;
#11844 = ORIENTED_EDGE ( 'NONE', *, *, #5044, .F. ) ;
#11845 = ORIENTED_EDGE ( 'NONE', *, *, #8083, .T. ) ;
#11847 = ORIENTED_EDGE ( 'NONE', *, *, #7675, .T. ) ;
#11846 = ADVANCED_FACE ( 'NONE', ( #11071, #3898 ), #19630, .T. ) ;
#11848 = VERTEX_POINT ( 'NONE', #8578 ) ;
#11849 = DIRECTION ( 'NONE',  ( 5.551115123125782702E-16, 1.201780285297635172E-31, -1.000000000000000000 ) ) ;
#11850 = LINE ( 'NONE', #2674, #3893 ) ;
#11851 = VERTEX_POINT ( 'NONE', #23177 ) ;
#11852 = EDGE_CURVE ( 'NONE', #4132, #955, #3179, .T. ) ;
#11853 = CARTESIAN_POINT ( 'NONE',  ( 77.42435809754140053, -6.999999999999811706, -5.999999999999984901 ) ) ;
#11854 = DIRECTION ( 'NONE',  ( -0.000000000000000000, 0.000000000000000000, -1.000000000000000000 ) ) ;
#11855 = DIRECTION ( 'NONE',  ( -0.000000000000000000, -0.000000000000000000, 1.000000000000000000 ) ) ;
#11856 = ORIENTED_EDGE ( 'NONE', *, *, #12723, .T. ) ;
#11857 = EDGE_CURVE ( 'NONE', #3142, #1999, #6901, .T. ) ;
#11858 = CARTESIAN_POINT ( 'NONE',  ( -6.130979318160965086, 35.99999999900384040, -18.86947933461498295 ) ) ;
#11859 = DIRECTION ( 'NONE',  ( 0.000000000000000000, 0.000000000000000000, 1.000000000000000000 ) ) ;
#11860 = DIRECTION ( 'NONE',  ( -1.000000000000000000, 0.000000000000000000, 0.000000000000000000 ) ) ;
#11861 = DIRECTION ( 'NONE',  ( -5.551115123561405253E-17, -1.000000000000000000, -2.256980353643891447E-27 ) ) ;
#11862 = FACE_OUTER_BOUND ( 'NONE', #18502, .T. ) ;
#11863 = AXIS2_PLACEMENT_3D ( 'NONE', #21093, #4959, #14025 ) ;
#11864 = DIRECTION ( 'NONE',  ( -9.693522803355793065E-26, 5.963788443470849249E-28, 1.000000000000000000 ) ) ;
#11865 = LINE ( 'NONE', #9875, #20561 ) ;
#11866 =( NAMED_UNIT ( * ) SI_UNIT ( $, .STERADIAN. ) SOLID_ANGLE_UNIT ( ) );
#11867 = CARTESIAN_POINT ( 'NONE',  ( -0.5000000000000975886, 4.799999999999929656, 7.500000000000007105 ) ) ;
#11868 = ORIENTED_EDGE ( 'NONE', *, *, #17044, .T. ) ;
#11869 = AXIS2_PLACEMENT_3D ( 'NONE', #9487, #13142, #2540 ) ;
#11870 = EDGE_LOOP ( 'NONE', ( #6567, #19308, #17328, #15100 ) ) ;
#11871 = EDGE_CURVE ( 'NONE', #1774, #14364, #12906, .T. ) ;
#11873 = EDGE_LOOP ( 'NONE', ( #21812, #11238 ) ) ;
#11872 = ORIENTED_EDGE ( 'NONE', *, *, #19155, .F. ) ;
#11874 = AXIS2_PLACEMENT_3D ( 'NONE', #577, #2218, #5642 ) ;
#11875 = CARTESIAN_POINT ( 'NONE',  ( 7.499999999999992895, -5.999999999999981348, 10.25000000000000888 ) ) ;
#11876 = EDGE_CURVE ( 'NONE', #919, #7321, #502, .T. ) ;
#11877 = CARTESIAN_POINT ( 'NONE',  ( -50.65685424949280247, 1.387778780781445676E-14, 8.000000000000090594 ) ) ;
#11878 =( GEOMETRIC_REPRESENTATION_CONTEXT ( 3 ) GLOBAL_UNCERTAINTY_ASSIGNED_CONTEXT ( ( #6036 ) ) GLOBAL_UNIT_ASSIGNED_CONTEXT ( ( #11281, #9295, #12817 ) ) REPRESENTATION_CONTEXT ( 'NONE', 'WORKASPACE' ) );
#11879 = LINE ( 'NONE', #13993, #18769 ) ;
#11880 = ORIENTED_EDGE ( 'NONE', *, *, #17014, .T. ) ;
#11881 = DIRECTION ( 'NONE',  ( -1.387778780781450803E-15, 0.000000000000000000, 1.000000000000000000 ) ) ;
#11882 = DIRECTION ( 'NONE',  ( -2.775557561562883647E-17, 3.406761633869147840E-16, -1.000000000000000000 ) ) ;
#11883 = DIRECTION ( 'NONE',  ( 0.000000000000000000, 0.000000000000000000, -1.000000000000000000 ) ) ;
#11884 = CARTESIAN_POINT ( 'NONE',  ( 3.349226789952567618, 2.685125164760785221, -0.2236248678334500084 ) ) ;
#11885 = CARTESIAN_POINT ( 'NONE',  ( -4.330127018922179438, 4.999999999999976907, -7.500000000000000000 ) ) ;
#11886 = DIRECTION ( 'NONE',  ( -2.775557561562891351E-14, 1.000000000000000000, 0.000000000000000000 ) ) ;
#11887 = CARTESIAN_POINT ( 'NONE',  ( 30.00000000029184832, 2.999999999003851503, -39.00000000000000000 ) ) ;
#11888 = AXIS2_PLACEMENT_3D ( 'NONE', #15610, #2805, #15147 ) ;
#11889 = CARTESIAN_POINT ( 'NONE',  ( 4.750000000000013323, 3.286685320581564807E-14, -1.500000000000001332 ) ) ;
#11890 = CARTESIAN_POINT ( 'NONE',  ( 0.000000000000000000, -1.750000000000025757, 4.749999999999973355 ) ) ;
#11891 = ORIENTED_EDGE ( 'NONE', *, *, #17135, .T. ) ;
#11892 = VECTOR ( 'NONE', #22429, 1000.000000000000000 ) ;
#11894 = ORIENTED_EDGE ( 'NONE', *, *, #17331, .F. ) ;
#11893 = ORIENTED_EDGE ( 'NONE', *, *, #5701, .T. ) ;
#11895 = ORIENTED_EDGE ( 'NONE', *, *, #1932, .T. ) ;
#11897 = EDGE_LOOP ( 'NONE', ( #7861, #15539, #17905, #11461 ) ) ;
#11896 = ORIENTED_EDGE ( 'NONE', *, *, #6808, .F. ) ;
#11898 = ORIENTED_EDGE ( 'NONE', *, *, #7242, .F. ) ;
#11899 = DIRECTION ( 'NONE',  ( -0.6819983600625061371, -0.7313537016191633544, 0.000000000000000000 ) ) ;
#11900 = CARTESIAN_POINT ( 'NONE',  ( -2.742413778650712342, -1.325747111984083793, 4.749999999999999112 ) ) ;
#11901 = DIRECTION ( 'NONE',  ( 2.013525853228507892E-32, 6.902532920683810383E-31, -1.000000000000000000 ) ) ;
#11902 = CARTESIAN_POINT ( 'NONE',  ( 66.26395429947839943, 0.000000000000000000, 6.000000000000178524 ) ) ;
#11903 = DIRECTION ( 'NONE',  ( -3.070652698126927723E-17, -1.000000000000000000, 4.167305704548413124E-17 ) ) ;
#11904 = AXIS2_PLACEMENT_3D ( 'NONE', #17676, #6997, #21349 ) ;
#11905 = DIRECTION ( 'NONE',  ( 1.000000000000000000, 0.000000000000000000, 0.000000000000000000 ) ) ;
#11906 = AXIS2_PLACEMENT_3D ( 'NONE', #4480, #4828, #11998 ) ;
#11907 = DIRECTION ( 'NONE',  ( -1.000000000000000000, -1.734723475976805517E-15, 0.000000000000000000 ) ) ;
#11908 = PLANE ( 'NONE',  #1093 ) ;
#11909 = FACE_OUTER_BOUND ( 'NONE', #20969, .T. ) ;
#11910 = FACE_OUTER_BOUND ( 'NONE', #21885, .T. ) ;
#11911 = ADVANCED_FACE ( 'NONE', ( #1523 ), #21933, .F. ) ;
#11912 = CARTESIAN_POINT ( 'NONE',  ( 22.49999999999998224, 2.000000000000001776, -2.081668171172168513E-14 ) ) ;
#11913 = VECTOR ( 'NONE', #17500, 1000.000000000000114 ) ;
#11914 = CARTESIAN_POINT ( 'NONE',  ( -8.113551354210013500, -12.41661007101923175, 7.426820295479667600 ) ) ;
#11915 = LINE ( 'NONE', #13580, #4415 ) ;
#11916 = CARTESIAN_POINT ( 'NONE',  ( 3.958476099525450209, -1.406653531810534430, -3.500000000000007105 ) ) ;
#11917 = ORIENTED_EDGE ( 'NONE', *, *, #2349, .T. ) ;
#11918 = PRODUCT_DEFINITION_CONTEXT ( 'detailed design', #3529, 'design' ) ;
#11919 = CIRCLE ( 'NONE', #14544, 4.750000000000013323 ) ;
#11921 = EDGE_LOOP ( 'NONE', ( #18795, #11263, #1157, #2552 ) ) ;
#11920 = ORIENTED_EDGE ( 'NONE', *, *, #16191, .T. ) ;
#11922 = VERTEX_POINT ( 'NONE', #14334 ) ;
#11923 = ORIENTED_EDGE ( 'NONE', *, *, #679, .T. ) ;
#11924 = EDGE_LOOP ( 'NONE', ( #19032, #1459, #18791, #9019 ) ) ;
#11925 = CIRCLE ( 'NONE', #10057, 0.5000000000000022204 ) ;
#11926 = ORIENTED_EDGE ( 'NONE', *, *, #19052, .T. ) ;
#11927 = DIRECTION ( 'NONE',  ( -2.775557561562883955E-17, 3.406761633869148826E-16, -1.000000000000000000 ) ) ;
#11928 = CIRCLE ( 'NONE', #4801, 6.000000000000000000 ) ;
#11929 = FACE_OUTER_BOUND ( 'NONE', #19138, .T. ) ;
#11930 = ORIENTED_EDGE ( 'NONE', *, *, #15118, .F. ) ;
#11931 = DIRECTION ( 'NONE',  ( 3.330669073875432643E-16, 4.437342591868153746E-31, -1.000000000000000000 ) ) ;
#11932 = TOROIDAL_SURFACE ( 'NONE', #2166, 5.384454397937119552, 0.5155456020628805813 ) ;
#11933 = CARTESIAN_POINT ( 'NONE',  ( -6.245004513516505540E-14, -4.862606272033144883, -3.745885042887461935 ) ) ;
#11934 = CARTESIAN_POINT ( 'NONE',  ( 4.114405500665262672, 2.025575754679666662, 3.508400121684944750 ) ) ;
#11935 = DIRECTION ( 'NONE',  ( -1.000000000000000000, -4.440892098500625176E-16, 0.000000000000000000 ) ) ;
#11936 = DIRECTION ( 'NONE',  ( -5.551115123561405253E-17, -1.000000000000000000, -2.256980353643891447E-27 ) ) ;
#11937 = CARTESIAN_POINT ( 'NONE',  ( 57.15235153779114796, -1.074585193523325266, -6.499999999999977796 ) ) ;
#11938 = AXIS2_PLACEMENT_3D ( 'NONE', #13464, #6180, #18636 ) ;
#11939 = EDGE_CURVE ( 'NONE', #12509, #22096, #3504, .T. ) ;
#11940 = DIRECTION ( 'NONE',  ( -1.454462294001240516E-30, -1.000000000000000000, 0.000000000000000000 ) ) ;
#11941 = CARTESIAN_POINT ( 'NONE',  ( -50.65685424949267457, -7.632783294297951215E-14, 8.000000000000047962 ) ) ;
#11942 = CARTESIAN_POINT ( 'NONE',  ( 0.3126073911696447549, 2.020725942163688504, -3.499999999999996003 ) ) ;
#11943 = PLANE ( 'NONE',  #7389 ) ;
#11944 = ORIENTED_EDGE ( 'NONE', *, *, #12894, .F. ) ;
#11945 = VECTOR ( 'NONE', #13294, 1000.000000000000000 ) ;
#11946 = ADVANCED_FACE ( 'NONE', ( #13981 ), #7060, .T. ) ;
#11947 = CARTESIAN_POINT ( 'NONE',  ( 4.180345304246196214, 4.135116856707401034, -0.02129519942689707401 ) ) ;
#11948 = AXIS2_PLACEMENT_3D ( 'NONE', #15297, #1421, #8596 ) ;
#11949 = PLANE ( 'NONE',  #20572 ) ;
#11950 = CIRCLE ( 'NONE', #23248, 4.999999999999999112 ) ;
#11951 = ADVANCED_FACE ( 'NONE', ( #17629 ), #5972, .F. ) ;
#11952 = VERTEX_POINT ( 'NONE', #16086 ) ;
#11953 = ADVANCED_FACE ( 'NONE', ( #17749 ), #10651, .T. ) ;
#11954 = ORIENTED_EDGE ( 'NONE', *, *, #8532, .T. ) ;
#11955 = ORIENTED_EDGE ( 'NONE', *, *, #19570, .F. ) ;
#11956 = ORIENTED_EDGE ( 'NONE', *, *, #3919, .T. ) ;
#11957 = DIRECTION ( 'NONE',  ( -2.013525853228507892E-32, -6.902532920683810383E-31, 1.000000000000000000 ) ) ;
#11958 = DIRECTION ( 'NONE',  ( 1.454462294001240516E-30, 1.000000000000000000, 0.000000000000000000 ) ) ;
#11959 = ORIENTED_EDGE ( 'NONE', *, *, #4211, .T. ) ;
#11960 = PLANE ( 'NONE',  #22256 ) ;
#11961 = DIRECTION ( 'NONE',  ( -0.9878135252003128475, 1.532010627492774680E-16, 0.1556420233463030045 ) ) ;
#11962 = DIRECTION ( 'NONE',  ( -2.775557561562883647E-17, 3.652049423109057473E-16, -1.000000000000000000 ) ) ;
#11963 = ADVANCED_FACE ( 'NONE', ( #21527 ), #5024, .T. ) ;
#11964 = AXIS2_PLACEMENT_3D ( 'NONE', #14099, #10454, #21639 ) ;
#11965 = DIRECTION ( 'NONE',  ( 1.000000000000000000, -4.190823558986610327E-31, 1.733449886265890494E-32 ) ) ;
#11966 = CARTESIAN_POINT ( 'NONE',  ( -6.958039891257955745, 36.00029345514013102, -26.50000000000000000 ) ) ;
#11967 = AXIS2_PLACEMENT_3D ( 'NONE', #22050, #14981, #20291 ) ;
#11968 = CARTESIAN_POINT ( 'NONE',  ( -7.573440241539831419, -0.1138337924791395506, 7.421600184846377068 ) ) ;
#11969 = DIRECTION ( 'NONE',  ( 0.9706398123736367234, 2.735793299299322016E-14, 0.2405376366294291746 ) ) ;
#11970 = CARTESIAN_POINT ( 'NONE',  ( 2.499999999999998668, 4.500000000000031974, -17.75000000000001776 ) ) ;
#11971 = ADVANCED_BREP_SHAPE_REPRESENTATION ( '', ( #12881, #22115 ), #2577 ) ;
#11972 = CARTESIAN_POINT ( 'NONE',  ( 0.000000000000000000, 7.999999999999983125, 0.000000000000000000 ) ) ;
#11973 = DIRECTION ( 'NONE',  ( 1.066786462891689527E-26, 6.656013887802287108E-31, 1.000000000000000000 ) ) ;
#11974 = EDGE_CURVE ( 'NONE', #1206, #9571, #1278, .T. ) ;
#11975 = CARTESIAN_POINT ( 'NONE',  ( -56.91911807125110556, 3.200000000000057021, -8.333333333333358794 ) ) ;
#11976 = EDGE_CURVE ( 'NONE', #20222, #9423, #3676, .T. ) ;
#11977 = DIRECTION ( 'NONE',  ( 1.333893503340774882E-15, 2.778352770573747380E-17, 1.000000000000000000 ) ) ;
#11978 = ORIENTED_EDGE ( 'NONE', *, *, #19344, .T. ) ;
#11979 = EDGE_CURVE ( 'NONE', #20776, #9332, #10281, .T. ) ;
#11980 = CIRCLE ( 'NONE', #14990, 4.500000000000045297 ) ;
#11981 = AXIS2_PLACEMENT_3D ( 'NONE', #21735, #18425, #9377 ) ;
#11982 = ORIENTED_EDGE ( 'NONE', *, *, #2329, .T. ) ;
#11984 = ORIENTED_EDGE ( 'NONE', *, *, #20586, .F. ) ;
#11983 = ORIENTED_EDGE ( 'NONE', *, *, #1779, .T. ) ;
#11985 = TOROIDAL_SURFACE ( 'NONE', #20285, 3.500000000000000888, 0.5000000000000000000 ) ;
#11986 = CARTESIAN_POINT ( 'NONE',  ( 0.3126073911695753660, -2.020725942163847932, -3.499999999999975131 ) ) ;
#11987 = COLOUR_RGB ( '', 0.66274510, 0.83137255, 0.94901961) ;
#11988 = FACE_OUTER_BOUND ( 'NONE', #11783, .T. ) ;
#11989 = ORIENTED_EDGE ( 'NONE', *, *, #7548, .T. ) ;
#11990 = DIRECTION ( 'NONE',  ( 2.220446049250313081E-16, -1.000000000000000000, 7.025792437124636392E-31 ) ) ;
#11991 = CARTESIAN_POINT ( 'NONE',  ( 3.951447005078450037, 1.347150628109081039, -3.499999999999995559 ) ) ;
#11992 = DIRECTION ( 'NONE',  ( -1.436734306171084565E-17, -0.2588190451025179084, -0.9659258262890690894 ) ) ;
#11993 = FACE_OUTER_BOUND ( 'NONE', #22672, .T. ) ;
#11994 = CARTESIAN_POINT ( 'NONE',  ( -43.10883117545714782, -4.565685424949276872, 7.500000000000062172 ) ) ;
#11995 = CARTESIAN_POINT ( 'NONE',  ( -55.05572809000125289, -0.5000000000001045830, -10.00000000000006395 ) ) ;
#11996 = CARTESIAN_POINT ( 'NONE',  ( 2.775557561562891351E-14, 10.99999999999998579, -3.000000000000002665 ) ) ;
#11997 = ADVANCED_FACE ( 'NONE', ( #8089 ), #15606, .F. ) ;
#11998 = DIRECTION ( 'NONE',  ( 1.000000000000000000, 2.282530889443153710E-16, 0.000000000000000000 ) ) ;
#11999 = CARTESIAN_POINT ( 'NONE',  ( -7.499999999999992895, -12.00000000000004263, 6.250000000000033751 ) ) ;
#12000 = CIRCLE ( 'NONE', #11631, 4.607329295533694413 ) ;
#12001 = DIRECTION ( 'NONE',  ( 1.066194817212772764E-26, 0.000000000000000000, 1.000000000000000000 ) ) ;
#12002 = EDGE_CURVE ( 'NONE', #18123, #1546, #20688, .T. ) ;
#12003 =( GEOMETRIC_REPRESENTATION_CONTEXT ( 3 ) GLOBAL_UNCERTAINTY_ASSIGNED_CONTEXT ( ( #18760 ) ) GLOBAL_UNIT_ASSIGNED_CONTEXT ( ( #20735, #22499, #6386 ) ) REPRESENTATION_CONTEXT ( 'NONE', 'WORKASPACE' ) );
#12004 = EDGE_LOOP ( 'NONE', ( #13168, #14883, #22233, #6907 ) ) ;
#12005 = DIRECTION ( 'NONE',  ( 1.110223024625156540E-16, 1.526556658859590243E-16, -1.000000000000000000 ) ) ;
#12007 = ORIENTED_EDGE ( 'NONE', *, *, #17720, .F. ) ;
#12006 = VERTEX_POINT ( 'NONE', #10092 ) ;
#12008 = ORIENTED_EDGE ( 'NONE', *, *, #19412, .F. ) ;
#12010 = EDGE_LOOP ( 'NONE', ( #20534, #4365, #17535, #11202, #4782, #17155, #6846, #11459 ) ) ;
#12009 = ORIENTED_EDGE ( 'NONE', *, *, #22875, .T. ) ;
#12011 = ORIENTED_EDGE ( 'NONE', *, *, #17007, .F. ) ;
#12012 = FACE_OUTER_BOUND ( 'NONE', #9647, .T. ) ;
#12013 = DIRECTION ( 'NONE',  ( -1.000000000000000000, -2.699383410053117892E-30, -3.885780586188017323E-16 ) ) ;
#12014 = CIRCLE ( 'NONE', #4865, 2.500000000000015987 ) ;
#12015 = CYLINDRICAL_SURFACE ( 'NONE', #11863, 2.550000000000003819 ) ;
#12016 = DIRECTION ( 'NONE',  ( -2.220446049250313081E-16, 1.000000000000000000, -7.025792437124636392E-31 ) ) ;
#12017 = CARTESIAN_POINT ( 'NONE',  ( -8.498922697886580835, -1.509195795641812499, 6.997949321565075209 ) ) ;
#12018 = FACE_OUTER_BOUND ( 'NONE', #11433, .T. ) ;
#12019 = CYLINDRICAL_SURFACE ( 'NONE', #12138, 2.000000000000015543 ) ;
#12020 = DIRECTION ( 'NONE',  ( 1.424116703980815236E-16, 1.000000000000000000, -6.902532920683853297E-31 ) ) ;
#12021 = DIRECTION ( 'NONE',  ( 3.254448077146059901E-32, 1.000000000000000000, 6.409494854920712161E-31 ) ) ;
#12022 = EDGE_CURVE ( 'NONE', #9917, #16719, #10668, .T. ) ;
#12023 = CARTESIAN_POINT ( 'NONE',  ( -4.000000000000004441, -1.549102112939104492, -0.1578953385959430966 ) ) ;
#12024 = CARTESIAN_POINT ( 'NONE',  ( 6.500000000000283329, 3.000000000000141220, -5.999999999999943157 ) ) ;
#12025 = DIRECTION ( 'NONE',  ( 1.000000000000000000, 5.328079247643017455E-14, 0.000000000000000000 ) ) ;
#12026 = APPLICATION_CONTEXT ( 'automotive_design' ) ;
#12027 = CARTESIAN_POINT ( 'NONE',  ( 4.086376042167604972, -1.979461949354206052, 3.571471332069173776 ) ) ;
#12028 = ADVANCED_FACE ( 'NONE', ( #22795, #18799 ), #20920, .F. ) ;
#12029 = EDGE_LOOP ( 'NONE', ( #21786, #1002, #11029 ) ) ;
#12030 =( LENGTH_UNIT ( ) NAMED_UNIT ( * ) SI_UNIT ( .MILLI., .METRE. ) );
#12031 = VECTOR ( 'NONE', #14028, 1000.000000000000000 ) ;
#12033 = ORIENTED_EDGE ( 'NONE', *, *, #14696, .F. ) ;
#12032 = ORIENTED_EDGE ( 'NONE', *, *, #14683, .F. ) ;
#12034 = EDGE_LOOP ( 'NONE', ( #22177, #4493, #19546, #10718 ) ) ;
#12035 = ORIENTED_EDGE ( 'NONE', *, *, #15004, .T. ) ;
#12036 = VERTEX_POINT ( 'NONE', #22334 ) ;
#12037 = EDGE_CURVE ( 'NONE', #2097, #15576, #11850, .T. ) ;
#12038 = ORIENTED_EDGE ( 'NONE', *, *, #3128, .T. ) ;
#12039 = DIRECTION ( 'NONE',  ( 0.2405376366294550983, 0.000000000000000000, -0.9706398123736303951 ) ) ;
#12040 = DIRECTION ( 'NONE',  ( -1.000000000000000000, 2.168404344971005170E-16, -1.203141491611682442E-30 ) ) ;
#12041 = ORIENTED_EDGE ( 'NONE', *, *, #20662, .T. ) ;
#12042 = CARTESIAN_POINT ( 'NONE',  ( 30.00000000029184832, 2.999999999003851503, -41.54999999999999716 ) ) ;
#12043 = DIRECTION ( 'NONE',  ( -1.331202777560457422E-30, -1.000000000000000000, 7.395570986446985676E-31 ) ) ;
#12044 = DIRECTION ( 'NONE',  ( 0.6819983600625073583, -0.7313537016191622442, -1.665472943098395307E-16 ) ) ;
#12045 = CARTESIAN_POINT ( 'NONE',  ( 1.999999999999992673, 3.464101615137806789, -3.142992957459250114 ) ) ;
#12046 = CIRCLE ( 'NONE', #2287, 7.500000000000001776 ) ;
#12047 = DIRECTION ( 'NONE',  ( -1.000000000000000000, -2.699383410053119644E-30, -3.330669073875432643E-16 ) ) ;
#12048 = DIRECTION ( 'NONE',  ( 0.000000000000000000, 0.000000000000000000, 1.000000000000000000 ) ) ;
#12049 = CARTESIAN_POINT ( 'NONE',  ( 1.369266385878512349, -1.008369684239886283E-15, -4.607329295533711289 ) ) ;
#12050 = PLANE ( 'NONE',  #20062 ) ;
#12051 = CARTESIAN_POINT ( 'NONE',  ( -7.629227790279464294, -1.952801550923857654, 8.369856247450591979 ) ) ;
#12052 = EDGE_LOOP ( 'NONE', ( #4779, #2611, #13734, #20379 ) ) ;
#12053 = DIRECTION ( 'NONE',  ( -0.000000000000000000, 1.000000000000000000, -0.000000000000000000 ) ) ;
#12054 = FACE_OUTER_BOUND ( 'NONE', #17070, .T. ) ;
#12056 = VERTEX_POINT ( 'NONE', #4313 ) ;
#12055 = ORIENTED_EDGE ( 'NONE', *, *, #22762, .F. ) ;
#12057 = ORIENTED_EDGE ( 'NONE', *, *, #7643, .T. ) ;
#12058 = AXIS2_PLACEMENT_3D ( 'NONE', #2334, #9518, #14921 ) ;
#12059 = AXIS2_PLACEMENT_3D ( 'NONE', #11033, #13036, #7624 ) ;
#12060 = ORIENTED_EDGE ( 'NONE', *, *, #18463, .T. ) ;
#12061 = ADVANCED_FACE ( 'NONE', ( #15250 ), #9530, .F. ) ;
#12062 = DIRECTION ( 'NONE',  ( -1.000000000000000000, 2.775557561562874627E-14, 0.000000000000000000 ) ) ;
#12063 = DIRECTION ( 'NONE',  ( -2.172745813409349776E-17, 1.000000000000000000, -1.309377075419428048E-16 ) ) ;
#12064 = LINE ( 'NONE', #6792, #15104 ) ;
#12065 = DIRECTION ( 'NONE',  ( 0.000000000000000000, 0.000000000000000000, -1.000000000000000000 ) ) ;
#12066 = CARTESIAN_POINT ( 'NONE',  ( -6.555066805945576033E-15, -12.15667283655308850, 12.14055452724117856 ) ) ;
#12067 = ADVANCED_FACE ( 'NONE', ( #20811 ), #16897, .T. ) ;
#12068 = FACE_OUTER_BOUND ( 'NONE', #15425, .T. ) ;
#12069 = CARTESIAN_POINT ( 'NONE',  ( 4.158806965674280320, 1.986429158307019938, 3.559403772175798952 ) ) ;
#12070 = CARTESIAN_POINT ( 'NONE',  ( 22.49999999999998224, 2.000000000000001776, -1.250000000000021982 ) ) ;
#12071 = ADVANCED_FACE ( 'NONE', ( #6217 ), #18940, .T. ) ;
#12072 = DIRECTION ( 'NONE',  ( -5.551115123561405253E-17, -1.000000000000000000, -2.256980353643891447E-27 ) ) ;
#12073 = CARTESIAN_POINT ( 'NONE',  ( 10.49999999999996803, -12.00000000000004796, 6.250000000000033751 ) ) ;
#12074 = AXIS2_PLACEMENT_3D ( 'NONE', #10070, #19120, #22896 ) ;
#12075 = TOROIDAL_SURFACE ( 'NONE', #16587, 4.500000000000000888, 0.5000000000000000000 ) ;
#12076 = DIRECTION ( 'NONE',  ( 5.551115123561405253E-17, 1.000000000000000000, -5.963788443470795439E-28 ) ) ;
#12077 = LINE ( 'NONE', #6693, #10794 ) ;
#12078 = CARTESIAN_POINT ( 'NONE',  ( -4.550510256924974684, 36.49999999900384751, -26.00000000000000000 ) ) ;
#12079 = CARTESIAN_POINT ( 'NONE',  ( 22.49999999999998224, 2.000000000000001776, -1.500000000000022204 ) ) ;
#12080 = ORIENTED_EDGE ( 'NONE', *, *, #19043, .T. ) ;
#12081 = EDGE_CURVE ( 'NONE', #6130, #18644, #5411, .T. ) ;
#12082 = AXIS2_PLACEMENT_3D ( 'NONE', #12732, #10849, #18148 ) ;
#12083 = ORIENTED_EDGE ( 'NONE', *, *, #2199, .T. ) ;
#12084 = ADVANCED_FACE ( 'NONE', ( #3032 ), #8795, .T. ) ;
#12085 = CARTESIAN_POINT ( 'NONE',  ( -4.775149780310945502, 35.99999999900384751, -25.50000003196489118 ) ) ;
#12087 = ORIENTED_EDGE ( 'NONE', *, *, #4642, .T. ) ;
#12086 = VERTEX_POINT ( 'NONE', #22684 ) ;
#12088 = VECTOR ( 'NONE', #22339, 1000.000000000000000 ) ;
#12089 = VERTEX_POINT ( 'NONE', #6571 ) ;
#12090 = FACE_OUTER_BOUND ( 'NONE', #2408, .T. ) ;
#12091 = AXIS2_PLACEMENT_3D ( 'NONE', #20457, #1162, #2676 ) ;
#12092 = ORIENTED_EDGE ( 'NONE', *, *, #10925, .F. ) ;
#12093 = AXIS2_PLACEMENT_3D ( 'NONE', #15835, #14319, #98 ) ;
#12094 = PLANE ( 'NONE',  #3225 ) ;
#12095 = AXIS2_PLACEMENT_3D ( 'NONE', #17362, #11957, #12062 ) ;
#12096 = CARTESIAN_POINT ( 'NONE',  ( -5.350349885510701675, 36.24720445779460931, -26.09137067849287206 ) ) ;
#12098 = ORIENTED_EDGE ( 'NONE', *, *, #21021, .T. ) ;
#12097 = ADVANCED_FACE ( 'NONE', ( #13738 ), #10196, .T. ) ;
#12099 = CARTESIAN_POINT ( 'NONE',  ( -64.00000000000045475, 0.5000000000000490719, -1.999999999999974021 ) ) ;
#12100 = DIRECTION ( 'NONE',  ( 0.000000000000000000, 0.000000000000000000, 1.000000000000000000 ) ) ;
#12101 = EDGE_CURVE ( 'NONE', #2293, #22503, #21506, .T. ) ;
#12102 = DIRECTION ( 'NONE',  ( 2.172745813409349776E-17, -1.000000000000000000, 1.309377075419428048E-16 ) ) ;
#12103 = PRODUCT_DEFINITION_SHAPE ( 'NONE', 'NONE',  #23273 ) ;
#12104 = ADVANCED_FACE ( 'NONE', ( #6915 ), #9024, .T. ) ;
#12105 = DIRECTION ( 'NONE',  ( 0.7071067811865474617, -0.7071067811865474617, 0.000000000000000000 ) ) ;
#12106 = CARTESIAN_POINT ( 'NONE',  ( -3.200000000000008171, -5.300000000000027356, -8.000000000000007105 ) ) ;
#12107 =( GEOMETRIC_REPRESENTATION_CONTEXT ( 3 ) GLOBAL_UNCERTAINTY_ASSIGNED_CONTEXT ( ( #6269 ) ) GLOBAL_UNIT_ASSIGNED_CONTEXT ( ( #14842, #5805, #4013 ) ) REPRESENTATION_CONTEXT ( 'NONE', 'WORKASPACE' ) );
#12108 = CARTESIAN_POINT ( 'NONE',  ( -4.000000000000003553, 2.309401076758532678, -5.242734410091827613 ) ) ;
#12109 = DIRECTION ( 'NONE',  ( 0.7071067811865535679, 0.7071067811865414665, 0.000000000000000000 ) ) ;
#12110 = FILL_AREA_STYLE ('',( #21076 ) ) ;
#12111 = CARTESIAN_POINT ( 'NONE',  ( 2.100000000000011635, -2.681188604469753282E-15, -4.999999999999998224 ) ) ;
#12112 = AXIS2_PLACEMENT_3D ( 'NONE', #11223, #3927, #11444 ) ;
#12113 = FILL_AREA_STYLE ('',( #8840 ) ) ;
#12114 = EDGE_CURVE ( 'NONE', #2883, #3085, #21951, .T. ) ;
#12115 = CIRCLE ( 'NONE', #17775, 6.249999999999992006 ) ;
#12116 = TOROIDAL_SURFACE ( 'NONE', #19636, 6.000000000000000888, 3.000000000000000000 ) ;
#12117 = EDGE_CURVE ( 'NONE', #13355, #16151, #4257, .T. ) ;
#12118 = EDGE_LOOP ( 'NONE', ( #9095, #12292, #89, #7885 ) ) ;
#12119 = CIRCLE ( 'NONE', #5747, 0.4999999999999995559 ) ;
#12120 = ADVANCED_FACE ( 'NONE', ( #3495 ), #6675, .T. ) ;
#12121 = EDGE_CURVE ( 'NONE', #14335, #21725, #7155, .T. ) ;
#12122 = DIRECTION ( 'NONE',  ( 0.5804539248959940112, 0.8142930928559051207, -1.997857000610750395E-16 ) ) ;
#12124 = ORIENTED_EDGE ( 'NONE', *, *, #643, .F. ) ;
#12123 = VERTEX_POINT ( 'NONE', #15828 ) ;
#12125 = VERTEX_POINT ( 'NONE', #4895 ) ;
#12127 = ORIENTED_EDGE ( 'NONE', *, *, #13063, .T. ) ;
#12126 = ORIENTED_EDGE ( 'NONE', *, *, #12128, .T. ) ;
#12128 = EDGE_CURVE ( 'NONE', #8379, #4761, #12542, .T. ) ;
#12129 = CARTESIAN_POINT ( 'NONE',  ( 4.050823680195217769, 2.400527758044860960, 2.978030508226152673 ) ) ;
#12130 = EDGE_CURVE ( 'NONE', #17301, #180, #15722, .T. ) ;
#12131 = CARTESIAN_POINT ( 'NONE',  ( 6.000000000291855429, -0.5000000009961480529, -5.999999999999998224 ) ) ;
#12132 = DIRECTION ( 'NONE',  ( -2.775557561562890735E-17, 3.352716401118095686E-16, -1.000000000000000000 ) ) ;
#12133 = EDGE_CURVE ( 'NONE', #12160, #18765, #5266, .T. ) ;
#12134 = CIRCLE ( 'NONE', #13644, 0.5000000000000019984 ) ;
#12135 = CARTESIAN_POINT ( 'NONE',  ( -95.20000000000061391, -9.714451465470119729E-14, 8.000000000000117240 ) ) ;
#12136 = TOROIDAL_SURFACE ( 'NONE', #1994, 5.500000000000000000, 0.5000000000000000000 ) ;
#12137 = FACE_OUTER_BOUND ( 'NONE', #21477, .T. ) ;
#12138 = AXIS2_PLACEMENT_3D ( 'NONE', #19556, #10154, #22864 ) ;
#12139 = DIRECTION ( 'NONE',  ( 2.013525853228508439E-32, 6.779273404243028164E-31, -1.000000000000000000 ) ) ;
#12140 = PRESENTATION_LAYER_ASSIGNMENT (  '', '', ( #10654 ) ) ;
#12141 = FACE_OUTER_BOUND ( 'NONE', #8262, .T. ) ;
#12142 = LINE ( 'NONE', #19328, #1261 ) ;
#12143 = DIRECTION ( 'NONE',  ( -4.844685039213900252E-16, -1.201780285297635172E-31, 1.000000000000000000 ) ) ;
#12144 = CARTESIAN_POINT ( 'NONE',  ( -95.20000000000067075, 2.700000000000014833, -1.999999999999974021 ) ) ;
#12145 = CYLINDRICAL_SURFACE ( 'NONE', #6307, 4.750000000000000888 ) ;
#12146 = CARTESIAN_POINT ( 'NONE',  ( 30.00000000029184832, -9.961476088449217059E-10, -5.999999999999998224 ) ) ;
#12147 = CARTESIAN_POINT ( 'NONE',  ( 61.48996577904083694, -5.119475911334187224, 6.500000000000130562 ) ) ;
#12148 = ORIENTED_EDGE ( 'NONE', *, *, #11736, .T. ) ;
#12149 = CIRCLE ( 'NONE', #23078, 0.5000000000000038858 ) ;
#12150 =( NAMED_UNIT ( * ) SI_UNIT ( $, .STERADIAN. ) SOLID_ANGLE_UNIT ( ) );
#12151 = CIRCLE ( 'NONE', #3519, 6.000000000000037303 ) ;
#12153 = ORIENTED_EDGE ( 'NONE', *, *, #19971, .T. ) ;
#12152 = VERTEX_POINT ( 'NONE', #12305 ) ;
#12154 = AXIS2_PLACEMENT_3D ( 'NONE', #14918, #16781, #22803 ) ;
#12155 = AXIS2_PLACEMENT_3D ( 'NONE', #20077, #3828, #22069 ) ;
#12156 = AXIS2_PLACEMENT_3D ( 'NONE', #4223, #4113, #12951 ) ;
#12157 = ORIENTED_EDGE ( 'NONE', *, *, #15485, .F. ) ;
#12158 = ORIENTED_EDGE ( 'NONE', *, *, #23171, .F. ) ;
#12159 = VERTEX_POINT ( 'NONE', #3155 ) ;
#12160 = VERTEX_POINT ( 'NONE', #10548 ) ;
#12161 = CARTESIAN_POINT ( 'NONE',  ( 114.8016533820240852, -5.880524088665822546, 6.000000000000123457 ) ) ;
#12162 = VERTEX_POINT ( 'NONE', #17650 ) ;
#12163 = DIRECTION ( 'NONE',  ( -1.000000000000000000, -2.699383410053119644E-30, -3.330669073875432643E-16 ) ) ;
#12164 = EDGE_CURVE ( 'NONE', #17995, #4397, #3390, .T. ) ;
#12165 = CARTESIAN_POINT ( 'NONE',  ( 0.000000000000000000, -14.99999999999997513, -1.387778780781445676E-14 ) ) ;
#12166 = VECTOR ( 'NONE', #4008, 1000.000000000000000 ) ;
#12167 = DIRECTION ( 'NONE',  ( -2.013525853228507892E-32, -6.902532920683810383E-31, 1.000000000000000000 ) ) ;
#12168 = VECTOR ( 'NONE', #7331, 1000.000000000000000 ) ;
#12169 = CARTESIAN_POINT ( 'NONE',  ( 3.951447005078448260, -2.357513599190994125, 2.916666666666669183 ) ) ;
#12170 = CARTESIAN_POINT ( 'NONE',  ( 119.5756419024615553, -11.00000000000006573, 6.500000000000012434 ) ) ;
#12171 = CARTESIAN_POINT ( 'NONE',  ( -2.500000000000015543, 3.191891195797327420E-15, -4.974600000000002353 ) ) ;
#12172 = AXIS2_PLACEMENT_3D ( 'NONE', #4287, #11466, #2531 ) ;
#12173 = CARTESIAN_POINT ( 'NONE',  ( 118.0000000000018190, -4.500000000000003553, 6.000000000000109246 ) ) ;
#12174 = DIRECTION ( 'NONE',  ( -0.8660254037844358210, 0.5000000000000046629, -1.141293895983254122E-15 ) ) ;
#12175 = CARTESIAN_POINT ( 'NONE',  ( -43.10883117545713361, 4.565685424949256443, 8.000000000000035527 ) ) ;
#12176 = DIRECTION ( 'NONE',  ( -1.000000000000000000, -5.598259082250514647E-17, -3.330669073875432643E-16 ) ) ;
#12177 = ORIENTED_EDGE ( 'NONE', *, *, #2663, .T. ) ;
#12178 = CARTESIAN_POINT ( 'NONE',  ( 4.050536630291685647, 2.401306687817039265, -2.976670123173765781 ) ) ;
#12179 = CARTESIAN_POINT ( 'NONE',  ( 88.75737332930587797, -11.02760560296348125, -6.000000000000067502 ) ) ;
#12181 = ORIENTED_EDGE ( 'NONE', *, *, #20591, .F. ) ;
#12180 = ORIENTED_EDGE ( 'NONE', *, *, #18849, .F. ) ;
#12182 = AXIS2_PLACEMENT_3D ( 'NONE', #9054, #8832, #23191 ) ;
#12183 = ORIENTED_EDGE ( 'NONE', *, *, #22086, .T. ) ;
#12184 = CIRCLE ( 'NONE', #9562, 4.749999999999981348 ) ;
#12185 = EDGE_LOOP ( 'NONE', ( #13610, #20863, #2852, #4314 ) ) ;
#12186 = DIRECTION ( 'NONE',  ( 0.000000000000000000, -6.938893903907237844E-15, -1.000000000000000000 ) ) ;
#12187 = DIRECTION ( 'NONE',  ( -3.885780586188016830E-16, -4.437342591868156373E-31, 1.000000000000000000 ) ) ;
#12188 = CARTESIAN_POINT ( 'NONE',  ( 2.500000000000002220, 1.124296205839700427E-14, -5.000000000000004441 ) ) ;
#12189 = CARTESIAN_POINT ( 'NONE',  ( -42.54314575050785407, -4.000000000000034639, -7.500000000000007105 ) ) ;
#12190 = DIRECTION ( 'NONE',  ( 1.000000000000000000, 0.000000000000000000, 2.668805347656601040E-16 ) ) ;
#12191 = DIRECTION ( 'NONE',  ( 0.000000000000000000, 1.000000000000000000, 0.000000000000000000 ) ) ;
#12192 = FACE_BOUND ( 'NONE', #22418, .T. ) ;
#12193 = FACE_OUTER_BOUND ( 'NONE', #6329, .T. ) ;
#12194 = DIRECTION ( 'NONE',  ( 0.000000000000000000, -6.162975822039153854E-31, -1.000000000000000000 ) ) ;
#12195 = DIRECTION ( 'NONE',  ( 5.551115123125782702E-16, 1.201780285297635172E-31, -1.000000000000000000 ) ) ;
#12196 = CONICAL_SURFACE ( 'NONE', #21988, 4.750000000000000888, 0.7853981633974430610 ) ;
#12197 = CARTESIAN_POINT ( 'NONE',  ( -65.00000000000052580, 0.5000000000000490719, 3.000000000000002665 ) ) ;
#12198 = CARTESIAN_POINT ( 'NONE',  ( 7.518994333257404072, -2.258039616118832971, 8.837702940568432197 ) ) ;
#12199 = DIRECTION ( 'NONE',  ( 1.000000000000000000, 6.224605580259554159E-31, -2.887593071917436153E-31 ) ) ;
#12200 = PRESENTATION_STYLE_ASSIGNMENT (( #15844 ) ) ;
#12201 = EDGE_CURVE ( 'NONE', #18645, #16059, #8908, .T. ) ;
#12202 = DIRECTION ( 'NONE',  ( -1.387778780781450803E-15, 0.000000000000000000, 1.000000000000000000 ) ) ;
#12203 = LINE ( 'NONE', #10564, #4792 ) ;
#12204 = ORIENTED_EDGE ( 'NONE', *, *, #10810, .T. ) ;
#12205 = ORIENTED_EDGE ( 'NONE', *, *, #766, .T. ) ;
#12206 = CARTESIAN_POINT ( 'NONE',  ( -5.631870895226652962, 35.99999999900384751, -25.73470486101134469 ) ) ;
#12208 = VERTEX_POINT ( 'NONE', #19607 ) ;
#12207 = VERTEX_POINT ( 'NONE', #13850 ) ;
#12209 = CIRCLE ( 'NONE', #13730, 6.500000000000023981 ) ;
#12210 = CARTESIAN_POINT ( 'NONE',  ( -2.742413778650615086, -1.325747111984059590, -4.749999999999997335 ) ) ;
#12211 = ORIENTED_EDGE ( 'NONE', *, *, #15622, .T. ) ;
#12212 = CARTESIAN_POINT ( 'NONE',  ( 3.680118525130219531, -2.494084732383396119, -0.3507732604232581819 ) ) ;
#12213 = CARTESIAN_POINT ( 'NONE',  ( -90.63385214007844581, 5.551115123125782702E-14, -7.926881151201908615 ) ) ;
#12214 = CARTESIAN_POINT ( 'NONE',  ( -42.54314575050785407, -4.800000000000019362, 8.000000000000007105 ) ) ;
#12215 = ORIENTED_EDGE ( 'NONE', *, *, #11383, .T. ) ;
#12216 = CARTESIAN_POINT ( 'NONE',  ( 5.773502691896191585, 4.999999999999984901, -4.999999999999999112 ) ) ;
#12217 = CARTESIAN_POINT ( 'NONE',  ( -56.54644007500113645, 0.5000000000000143219, -8.666666666666710483 ) ) ;
#12218 = CARTESIAN_POINT ( 'NONE',  ( 37.86602540378466841, 0.5000000000000004441, -6.499999999999992006 ) ) ;
#12219 = CARTESIAN_POINT ( 'NONE',  ( -7.554637128289425796, -13.87985946887537558, 7.453047528892608575 ) ) ;
#12220 = EDGE_CURVE ( 'NONE', #9565, #7514, #16647, .T. ) ;
#12221 = FACE_OUTER_BOUND ( 'NONE', #1209, .T. ) ;
#12222 = DIRECTION ( 'NONE',  ( 0.000000000000000000, 6.802837160693368935E-15, 1.000000000000000000 ) ) ;
#12223 = CARTESIAN_POINT ( 'NONE',  ( 3.958484000407217707, -2.327740518749036092, 2.968235154689960797 ) ) ;
#12224 = ADVANCED_FACE ( 'NONE', ( #5018 ), #21034, .F. ) ;
#12225 = FACE_OUTER_BOUND ( 'NONE', #14887, .T. ) ;
#12226 = ORIENTED_EDGE ( 'NONE', *, *, #17678, .F. ) ;
#12227 = EDGE_CURVE ( 'NONE', #20741, #2357, #7036, .T. ) ;
#12228 = AXIS2_PLACEMENT_3D ( 'NONE', #14604, #1890, #11066 ) ;
#12229 = DIRECTION ( 'NONE',  ( 0.8157488175929878960, -0.5784063161788965957, 2.220446049250313081E-16 ) ) ;
#12230 = EDGE_CURVE ( 'NONE', #14402, #16051, #1386, .T. ) ;
#12232 = EDGE_LOOP ( 'NONE', ( #22789, #7792, #13011, #1040 ) ) ;
#12231 = ORIENTED_EDGE ( 'NONE', *, *, #9739, .F. ) ;
#12233 = STYLED_ITEM ( 'NONE', ( #12200 ), #21257 ) ;
#12234 = EDGE_LOOP ( 'NONE', ( #3462, #10621, #23242, #13181 ) ) ;
#12236 = ORIENTED_EDGE ( 'NONE', *, *, #21821, .F. ) ;
#12235 = EDGE_LOOP ( 'NONE', ( #3113, #4573, #22825, #10879 ) ) ;
#12237 = CARTESIAN_POINT ( 'NONE',  ( 4.175002511812132333, 2.208363329454923640, -3.469254087858248514 ) ) ;
#12238 = CARTESIAN_POINT ( 'NONE',  ( -0.5000000000000559552, -1.999999999999988010, -7.500000000000007105 ) ) ;
#12239 = DIRECTION ( 'NONE',  ( -9.121204216617949000E-31, -1.000000000000000000, 6.982962677686261977E-15 ) ) ;
#12240 = DIRECTION ( 'NONE',  ( -1.000000000000000000, 5.551115122690166315E-17, 1.001543066815839268E-16 ) ) ;
#12241 = LINE ( 'NONE', #6987, #18426 ) ;
#12242 = EDGE_CURVE ( 'NONE', #12089, #8376, #15531, .T. ) ;
#12243 = CARTESIAN_POINT ( 'NONE',  ( 118.0000000000017195, -4.000000000000003553, 6.500000000000130562 ) ) ;
#12245 = EDGE_CURVE ( 'NONE', #8077, #3149, #20195, .T. ) ;
#12244 = SURFACE_SIDE_STYLE ('',( #159 ) ) ;
#12246 = EDGE_CURVE ( 'NONE', #3554, #283, #12776, .T. ) ;
#12247 = DIRECTION ( 'NONE',  ( 0.000000000000000000, 0.000000000000000000, -1.000000000000000000 ) ) ;
#12248 = VECTOR ( 'NONE', #9399, 1000.000000000000000 ) ;
#12249 = DIRECTION ( 'NONE',  ( 0.000000000000000000, 0.000000000000000000, 1.000000000000000000 ) ) ;
#12250 = CARTESIAN_POINT ( 'NONE',  ( 2.775557561562891351E-14, 2.999999999999992450, -0.4999999999999865663 ) ) ;
#12251 = DIRECTION ( 'NONE',  ( -1.000000000000000000, -4.440892098500626162E-16, 5.551115123125782702E-16 ) ) ;
#12252 = VECTOR ( 'NONE', #4664, 1000.000000000000000 ) ;
#12253 = DIRECTION ( 'NONE',  ( 1.733449886265891589E-32, -4.190823558986610327E-31, 1.000000000000000000 ) ) ;
#12254 = CARTESIAN_POINT ( 'NONE',  ( -8.954763739086851970, -12.50000000000002132, 6.678571428571506097 ) ) ;
#12255 = DIRECTION ( 'NONE',  ( 1.000000000000000000, 0.000000000000000000, 0.000000000000000000 ) ) ;
#12256 = EDGE_CURVE ( 'NONE', #16051, #9575, #8417, .T. ) ;
#12257 = LINE ( 'NONE', #8867, #16765 ) ;
#12258 = ORIENTED_EDGE ( 'NONE', *, *, #12117, .T. ) ;
#12259 = ADVANCED_FACE ( 'NONE', ( #19957 ), #21960, .T. ) ;
#12260 =( LENGTH_UNIT ( ) NAMED_UNIT ( * ) SI_UNIT ( .MILLI., .METRE. ) );
#12262 = EDGE_LOOP ( 'NONE', ( #6842, #200, #17097, #4190 ) ) ;
#12261 = ORIENTED_EDGE ( 'NONE', *, *, #19638, .T. ) ;
#12263 = EDGE_CURVE ( 'NONE', #3634, #9737, #22315, .T. ) ;
#12264 = ORIENTED_EDGE ( 'NONE', *, *, #1455, .F. ) ;
#12265 = AXIS2_PLACEMENT_3D ( 'NONE', #2916, #11961, #19144 ) ;
#12266 = ORIENTED_EDGE ( 'NONE', *, *, #4461, .T. ) ;
#12267 = EDGE_CURVE ( 'NONE', #7689, #9100, #3718, .T. ) ;
#12268 = EDGE_LOOP ( 'NONE', ( #12741, #15103, #9473, #17164 ) ) ;
#12269 = VECTOR ( 'NONE', #18963, 1000.000000000000000 ) ;
#12270 = ORIENTED_EDGE ( 'NONE', *, *, #23074, .T. ) ;
#12271 = CARTESIAN_POINT ( 'NONE',  ( 108.2426266706972058, -6.527605602963671316, -6.500000000000019540 ) ) ;
#12272 = PRESENTATION_LAYER_ASSIGNMENT (  '', '', ( #267 ) ) ;
#12273 = AXIS2_PLACEMENT_3D ( 'NONE', #15407, #21405, #13540 ) ;
#12274 = CARTESIAN_POINT ( 'NONE',  ( 0.000000000000000000, -4.618802153517061804, -5.600000000000000533 ) ) ;
#12275 = VERTEX_POINT ( 'NONE', #19842 ) ;
#12276 = CARTESIAN_POINT ( 'NONE',  ( -7.733764002503169088, -13.25269934883866263, 8.082002268151521562 ) ) ;
#12277 = DIRECTION ( 'NONE',  ( -1.000000000000000000, -0.000000000000000000, -0.000000000000000000 ) ) ;
#12278 = AXIS2_PLACEMENT_3D ( 'NONE', #12672, #12199, #6931 ) ;
#12279 = CARTESIAN_POINT ( 'NONE',  ( -95.20000000000064233, 0.5000000000000073275, 1.000000000000014655 ) ) ;
#12280 = CARTESIAN_POINT ( 'NONE',  ( -3.111695183146356892E-17, -14.99999999999997513, 4.749999999999985789 ) ) ;
#12281 = CARTESIAN_POINT ( 'NONE',  ( -8.954763739086851970, -0.5000000000000004441, 6.678571428571422608 ) ) ;
#12282 = FACE_OUTER_BOUND ( 'NONE', #276, .T. ) ;
#12283 = DIRECTION ( 'NONE',  ( 1.454462294001240516E-30, 1.000000000000000000, 0.000000000000000000 ) ) ;
#12284 = LINE ( 'NONE', #17347, #19586 ) ;
#12285 = CARTESIAN_POINT ( 'NONE',  ( -42.54314575050793934, -5.300000000000020250, 7.500000000000062172 ) ) ;
#12286 = DIRECTION ( 'NONE',  ( -1.000000000000000000, -2.699383410053119644E-30, -3.330669073875432643E-16 ) ) ;
#12287 = CIRCLE ( 'NONE', #12681, 2.550000000000003819 ) ;
#12288 = B_SPLINE_CURVE_WITH_KNOTS ( 'NONE', 3,
 ( #14243, #17768, #1988, #6833, #3754, #14475 ),
 .UNSPECIFIED., .F., .F.,
 ( 4, 2, 4 ),
 ( 0.000000000000000000, 0.0002095117440854730128, 0.0004190234881709460255 ),
 .UNSPECIFIED. ) ;
#12289 = ADVANCED_FACE ( 'NONE', ( #10887 ), #16406, .T. ) ;
#12290 = CARTESIAN_POINT ( 'NONE',  ( -3.499999999708153453, 2.999999999003851503, -19.00000000000000355 ) ) ;
#12291 = VECTOR ( 'NONE', #3147, 1000.000000000000000 ) ;
#12292 = ORIENTED_EDGE ( 'NONE', *, *, #8505, .F. ) ;
#12293 = FACE_OUTER_BOUND ( 'NONE', #15510, .T. ) ;
#12294 = CARTESIAN_POINT ( 'NONE',  ( -3.999999999708139686, 13.32455531934060744, -29.00000000000000355 ) ) ;
#12296 = VERTEX_POINT ( 'NONE', #7377 ) ;
#12295 = ORIENTED_EDGE ( 'NONE', *, *, #7168, .F. ) ;
#12297 = CIRCLE ( 'NONE', #5932, 0.5000000000000038858 ) ;
#12298 = ADVANCED_FACE ( 'NONE', ( #7488 ), #3544, .T. ) ;
#12299 = AXIS2_PLACEMENT_3D ( 'NONE', #5860, #16884, #6202 ) ;
#12300 = VECTOR ( 'NONE', #7677, 1000.000000000000000 ) ;
#12301 = ORIENTED_EDGE ( 'NONE', *, *, #14747, .T. ) ;
#12302 = ORIENTED_EDGE ( 'NONE', *, *, #12659, .T. ) ;
#12303 = PRODUCT ( 'MAS-693', 'MAS-693', '', ( #3352 ) ) ;
#12304 = DIRECTION ( 'NONE',  ( 1.454462294001240516E-30, 1.000000000000000000, 0.000000000000000000 ) ) ;
#12305 = CARTESIAN_POINT ( 'NONE',  ( 35.50000000029184832, -9.961476088449217059E-10, -26.00000000000000000 ) ) ;
#12306 = TOROIDAL_SURFACE ( 'NONE', #1065, 3.500000000000000888, 0.5000000000000000000 ) ;
#12307 = CARTESIAN_POINT ( 'NONE',  ( 7.135462137692308706E-16, -1.618211776087849834E-15, 4.750000000000013323 ) ) ;
#12308 = DIRECTION ( 'NONE',  ( 1.000000000000000000, -4.615739097524200579E-16, 1.134196829589822059E-15 ) ) ;
#12309 = VECTOR ( 'NONE', #15671, 1000.000000000000000 ) ;
#12310 = CYLINDRICAL_SURFACE ( 'NONE', #9109, 0.4999999999999995559 ) ;
#12311 = DIRECTION ( 'NONE',  ( 0.000000000000000000, 1.000000000000000000, 0.000000000000000000 ) ) ;
#12312 = FACE_OUTER_BOUND ( 'NONE', #21114, .T. ) ;
#12313 = CARTESIAN_POINT ( 'NONE',  ( -8.204963667274123296, -0.08625821904939658114, 7.312308861538882709 ) ) ;
#12314 = DIRECTION ( 'NONE',  ( 0.000000000000000000, 0.000000000000000000, 1.000000000000000000 ) ) ;
#12315 = DIRECTION ( 'NONE',  ( 0.000000000000000000, 0.000000000000000000, 1.000000000000000000 ) ) ;
#12316 = CARTESIAN_POINT ( 'NONE',  ( 3.973110223767139626, 2.264800795684280898E-11, 3.565797985667429781 ) ) ;
#12317 = AXIS2_PLACEMENT_3D ( 'NONE', #6603, #19184, #6720 ) ;
#12318 = AXIS2_PLACEMENT_3D ( 'NONE', #4876, #3131, #7953 ) ;
#12319 = CARTESIAN_POINT ( 'NONE',  ( -47.82842712474642610, -4.371572875253856516, 8.000000000000076383 ) ) ;
#12320 = FACE_OUTER_BOUND ( 'NONE', #8724, .T. ) ;
#12321 = DIRECTION ( 'NONE',  ( 0.000000000000000000, 0.000000000000000000, -1.000000000000000000 ) ) ;
#12322 = B_SPLINE_CURVE_WITH_KNOTS ( 'NONE', 3,
 ( #18340, #11272, #10174, #22771, #16550, #13826 ),
 .UNSPECIFIED., .F., .F.,
 ( 4, 2, 4 ),
 ( 0.01308430721348209473, 0.01410661710602284513, 0.01512892699856359380 ),
 .UNSPECIFIED. ) ;
#12323 = DIRECTION ( 'NONE',  ( 1.550910762415566494E-16, 1.000000000000000000, -8.135128085091684243E-31 ) ) ;
#12324 = DIRECTION ( 'NONE',  ( -1.000000000000000000, -1.479114197289387852E-30, 2.013525853228518840E-32 ) ) ;
#12325 = EDGE_LOOP ( 'NONE', ( #16976, #6419 ) ) ;
#12326 = ORIENTED_EDGE ( 'NONE', *, *, #18662, .F. ) ;
#12327 = CARTESIAN_POINT ( 'NONE',  ( -4.550510256924972907, 36.49999999900384751, -26.00000000000000000 ) ) ;
#12328 = AXIS2_PLACEMENT_3D ( 'NONE', #10903, #8689, #1516 ) ;
#12330 = ORIENTED_EDGE ( 'NONE', *, *, #21029, .T. ) ;
#12329 = ORIENTED_EDGE ( 'NONE', *, *, #5663, .T. ) ;
#12331 = AXIS2_PLACEMENT_3D ( 'NONE', #7929, #20408, #6408 ) ;
#12332 = CIRCLE ( 'NONE', #23265, 2.550000000000024691 ) ;
#12333 = DIRECTION ( 'NONE',  ( 2.220446049250313081E-16, -1.000000000000000000, 7.025792437124636392E-31 ) ) ;
#12334 = FACE_OUTER_BOUND ( 'NONE', #21066, .T. ) ;
#12335 = EDGE_CURVE ( 'NONE', #17392, #10026, #14538, .T. ) ;
#12336 = CARTESIAN_POINT ( 'NONE',  ( -6.999999999708156118, 6.999999999003851947, -19.00000000000000355 ) ) ;
#12337 = ORIENTED_EDGE ( 'NONE', *, *, #23080, .T. ) ;
#12338 = CARTESIAN_POINT ( 'NONE',  ( -91.02295700146251534, -3.200000000000101874, 6.338518968055054437 ) ) ;
#12339 = DIRECTION ( 'NONE',  ( -2.013525853228507892E-32, -6.902532920683810383E-31, 1.000000000000000000 ) ) ;
#12340 = CARTESIAN_POINT ( 'NONE',  ( 0.03027795055833982368, 0.6888063905328563052, -3.500000000000008882 ) ) ;
#12341 = DIRECTION ( 'NONE',  ( 1.424116703980815236E-16, 1.000000000000000000, -6.902532920683853297E-31 ) ) ;
#12342 = STYLED_ITEM ( 'NONE', ( #1264 ), #8352 ) ;
#12343 = DIRECTION ( 'NONE',  ( 0.1556420233463076119, 0.000000000000000000, 0.9878135252003121813 ) ) ;
#12344 = CARTESIAN_POINT ( 'NONE',  ( -4.000000000000087041, -2.309401076758553550, -0.5000000000000004441 ) ) ;
#12345 = DIRECTION ( 'NONE',  ( -1.066788928082016908E-26, -3.471809175856251779E-58, 1.000000000000000000 ) ) ;
#12346 = VECTOR ( 'NONE', #4580, 1000.000000000000000 ) ;
#12347 = CARTESIAN_POINT ( 'NONE',  ( 2.918498775983380256E-10, -9.961476088449217059E-10, 0.000000000000000000 ) ) ;
#12348 = DIRECTION ( 'NONE',  ( 0.000000000000000000, 3.382522293539642681E-32, 1.000000000000000000 ) ) ;
#12349 = TOROIDAL_SURFACE ( 'NONE', #18761, 9.499999999999998224, 0.5000000000000000000 ) ;
#12350 = CIRCLE ( 'NONE', #10481, 2.550000000000010481 ) ;
#12351 = CARTESIAN_POINT ( 'NONE',  ( 1.218648372641069717E-15, 1.875287567046784119E-16, 4.500000000000000000 ) ) ;
#12352 = CYLINDRICAL_SURFACE ( 'NONE', #11572, 0.2500000000000002220 ) ;
#12353 = EDGE_LOOP ( 'NONE', ( #11240, #21141, #3767, #21958 ) ) ;
#12354 = DIRECTION ( 'NONE',  ( -0.4724806060251043882, -0.6628221078245827291, 0.5808863316597552284 ) ) ;
#12356 = ORIENTED_EDGE ( 'NONE', *, *, #22939, .T. ) ;
#12355 = ORIENTED_EDGE ( 'NONE', *, *, #23239, .F. ) ;
#12357 = PRESENTATION_LAYER_ASSIGNMENT (  '', '', ( #357 ) ) ;
#12358 = ORIENTED_EDGE ( 'NONE', *, *, #3629, .F. ) ;
#12359 = ADVANCED_FACE ( 'NONE', ( #18307 ), #9478, .T. ) ;
#12361 = EDGE_LOOP ( 'NONE', ( #284, #5614, #13470, #21474 ) ) ;
#12360 = ORIENTED_EDGE ( 'NONE', *, *, #20352, .T. ) ;
#12362 = FACE_OUTER_BOUND ( 'NONE', #21382, .T. ) ;
#12363 = CARTESIAN_POINT ( 'NONE',  ( -12.84999999999999964, -12.00000000000002842, 5.750000000000018652 ) ) ;
#12364 = ADVANCED_FACE ( 'NONE', ( #9600 ), #428, .F. ) ;
#12365 = DIRECTION ( 'NONE',  ( 0.000000000000000000, 0.8381404052084411305, -0.5454545454545505212 ) ) ;
#12366 = CIRCLE ( 'NONE', #7492, 2.999999999999995559 ) ;
#12367 = FACE_OUTER_BOUND ( 'NONE', #16828, .T. ) ;
#12368 = CARTESIAN_POINT ( 'NONE',  ( 12.84999999999997300, 0.000000000000000000, -2.549999999999986944 ) ) ;
#12369 = CARTESIAN_POINT ( 'NONE',  ( -7.271441198316176191, -0.2709289393878913099, 8.039702399269740951 ) ) ;
#12370 = DIRECTION ( 'NONE',  ( -1.000000000000000000, 4.190823558986610327E-31, -1.733449886265890494E-32 ) ) ;
#12371 = FACE_OUTER_BOUND ( 'NONE', #9766, .T. ) ;
#12372 = CARTESIAN_POINT ( 'NONE',  ( 5.600000000000000533, -2.020725942163709377, -3.500000000000010214 ) ) ;
#12373 = ADVANCED_FACE ( 'NONE', ( #1946 ), #14433, .T. ) ;
#12374 = DIRECTION ( 'NONE',  ( 1.333893503340774882E-15, 2.778352770573747380E-17, 1.000000000000000000 ) ) ;
#12376 = EDGE_CURVE ( 'NONE', #8151, #15365, #13015, .T. ) ;
#12375 = AXIS2_PLACEMENT_3D ( 'NONE', #9171, #17878, #7181 ) ;
#12377 = FACE_OUTER_BOUND ( 'NONE', #9923, .T. ) ;
#12378 = ADVANCED_FACE ( 'NONE', ( #7601 ), #16305, .T. ) ;
#12379 = CARTESIAN_POINT ( 'NONE',  ( -55.05572809000125289, -1.179611963664228824E-13, -10.00000000000006395 ) ) ;
#12380 = DIRECTION ( 'NONE',  ( 1.000000000000000000, 4.972873964466789154E-14, 3.854941057726193231E-16 ) ) ;
#12381 = CARTESIAN_POINT ( 'NONE',  ( -4.204114297095823183, 1.660363174096529892, -3.602136431857980270 ) ) ;
#12382 = CARTESIAN_POINT ( 'NONE',  ( 4.086262629614028086, -4.082406995609982658, -0.07093633357110609716 ) ) ;
#12383 = ORIENTED_EDGE ( 'NONE', *, *, #9498, .T. ) ;
#12384 = APPLICATION_PROTOCOL_DEFINITION ( 'draft international standard', 'automotive_design', 1998, #9083 ) ;
#12386 = ORIENTED_EDGE ( 'NONE', *, *, #8990, .T. ) ;
#12385 = VERTEX_POINT ( 'NONE', #2296 ) ;
#12387 = VERTEX_POINT ( 'NONE', #4066 ) ;
#12388 = EDGE_CURVE ( 'NONE', #18942, #10463, #8431, .T. ) ;
#12389 = ADVANCED_FACE ( 'NONE', ( #206 ), #1296, .T. ) ;
#12391 = ORIENTED_EDGE ( 'NONE', *, *, #13106, .F. ) ;
#12390 = ORIENTED_EDGE ( 'NONE', *, *, #2753, .T. ) ;
#12392 = AXIS2_PLACEMENT_3D ( 'NONE', #10064, #2772, #19115 ) ;
#12393 = ORIENTED_EDGE ( 'NONE', *, *, #4021, .T. ) ;
#12394 = VERTEX_POINT ( 'NONE', #8182 ) ;
#12395 = EDGE_CURVE ( 'NONE', #17297, #8438, #22221, .T. ) ;
#12396 = ORIENTED_EDGE ( 'NONE', *, *, #6362, .F. ) ;
#12397 = DIRECTION ( 'NONE',  ( -1.000000000000000000, 0.000000000000000000, -2.668805347656595124E-16 ) ) ;
#12398 = DIRECTION ( 'NONE',  ( 0.000000000000000000, -6.938893903907174735E-15, 1.000000000000000000 ) ) ;
#12399 = CARTESIAN_POINT ( 'NONE',  ( -12.84999999999999964, -2.000000000000001776, 5.750000000000005329 ) ) ;
#12400 = CARTESIAN_POINT ( 'NONE',  ( 0.2499999999999655276, 2.000000000000015543, -2.000000000000001776 ) ) ;
#12401 = EDGE_CURVE ( 'NONE', #6728, #927, #12670, .T. ) ;
#12402 = DIRECTION ( 'NONE',  ( 2.168404344971005170E-16, 1.000000000000000000, -8.696324126752285467E-47 ) ) ;
#12403 = DIRECTION ( 'NONE',  ( 0.000000000000000000, -1.000000000000000000, 0.000000000000000000 ) ) ;
#12404 = CARTESIAN_POINT ( 'NONE',  ( -1.318389841742373392E-16, 1.618211776087849834E-15, -4.750000000000013323 ) ) ;
#12405 = CARTESIAN_POINT ( 'NONE',  ( 2.918498775983380256E-10, 6.999999999003851947, -26.00000000000000000 ) ) ;
#12406 = DIRECTION ( 'NONE',  ( -1.000000000000000000, -2.699383410053119644E-30, -3.330669073875432643E-16 ) ) ;
#12407 = DIRECTION ( 'NONE',  ( 0.9706398123736299510, 1.232595164407823064E-30, 0.2405376366294566526 ) ) ;
#12408 = CIRCLE ( 'NONE', #2272, 0.2500000000000000000 ) ;
#12409 = DIRECTION ( 'NONE',  ( 0.000000000000000000, 0.000000000000000000, 1.000000000000000000 ) ) ;
#12410 = DIRECTION ( 'NONE',  ( -1.000000000000000000, 4.615739097524200579E-16, -1.134196829589822059E-15 ) ) ;
#12411 =( BOUNDED_SURFACE ( )  B_SPLINE_SURFACE ( 3, 2, ( 
 ( #17477, #20556, #4425 ),
 ( #2901, #1033, #9845 ),
 ( #3146, #21023, #13729 ),
 ( #9970, #4888, #6437 ),
 ( #17119, #6665, #1380 ),
 ( #15239, #1150, #11947 ) ),
 .UNSPECIFIED., .F., .F., .F. ) 
 B_SPLINE_SURFACE_WITH_KNOTS ( ( 4, 2, 4 ),
 ( 3, 3 ),
 ( 0.01651999345535505592, 0.01858032176739835006, 0.02064065007944164767 ),
 ( 0.000000000000000000, 1.000000000000000000 ),
 .UNSPECIFIED. ) 
 GEOMETRIC_REPRESENTATION_ITEM ( )  RATIONAL_B_SPLINE_SURFACE ( (
 ( 1.000000000000000000, 0.8047781103519393575, 1.000000000000000000),
 ( 1.000000000000000000, 0.8123785825606938404, 1.000000000000000000),
 ( 1.000000000000000000, 0.8190671539784832866, 1.000000000000000000),
 ( 1.000000000000000000, 0.8192352254838310976, 1.000000000000000000),
 ( 1.000000000000000000, 0.8126129677209011914, 1.000000000000000000),
 ( 1.000000000000000000, 0.8047712537969730073, 1.000000000000000000) ) ) 
 REPRESENTATION_ITEM ( '' )  SURFACE ( )  );
#12412 = ORIENTED_EDGE ( 'NONE', *, *, #1086, .T. ) ;
#12413 = SURFACE_SIDE_STYLE ('',( #19596 ) ) ;
#12414 = DIRECTION ( 'NONE',  ( 1.000000000000000000, 4.252453317207022018E-31, -5.551115123125818447E-17 ) ) ;
#12415 = CARTESIAN_POINT ( 'NONE',  ( 88.75737332930596324, -6.527605602963476805, 6.000000000000165201 ) ) ;
#12417 = ORIENTED_EDGE ( 'NONE', *, *, #13406, .F. ) ;
#12416 = ORIENTED_EDGE ( 'NONE', *, *, #9869, .T. ) ;
#12418 = ADVANCED_FACE ( 'NONE', ( #22652, #16872 ), #20782, .F. ) ;
#12419 = EDGE_CURVE ( 'NONE', #3579, #5105, #4759, .T. ) ;
#12420 = ORIENTED_EDGE ( 'NONE', *, *, #4398, .T. ) ;
#12421 = ORIENTED_EDGE ( 'NONE', *, *, #10813, .F. ) ;
#12422 = VERTEX_POINT ( 'NONE', #15222 ) ;
#12423 = VERTEX_POINT ( 'NONE', #2881 ) ;
#12424 = DIRECTION ( 'NONE',  ( 3.032184104443272185E-30, 1.000000000000000000, -7.395570986447005381E-32 ) ) ;
#12425 = AXIS2_PLACEMENT_3D ( 'NONE', #19178, #10348, #20952 ) ;
#12426 = CARTESIAN_POINT ( 'NONE',  ( 42.00000000000014921, 10.49999999999999822, -0.4999999999999449329 ) ) ;
#12427 = EDGE_CURVE ( 'NONE', #6445, #15071, #3005, .T. ) ;
#12428 = CARTESIAN_POINT ( 'NONE',  ( 4.030867648403866355, 2.329326259789088915, -2.965488570641591881 ) ) ;
#12429 = CARTESIAN_POINT ( 'NONE',  ( 0.000000000000000000, 0.000000000000000000, 0.000000000000000000 ) ) ;
#12430 = DIRECTION ( 'NONE',  ( -9.121204216617949000E-31, -1.000000000000000000, 6.982962677686261977E-15 ) ) ;
#12431 = DIRECTION ( 'NONE',  ( 6.938893903907224433E-16, 1.201780285297635172E-31, -1.000000000000000000 ) ) ;
#12432 = DIRECTION ( 'NONE',  ( -0.000000000000000000, 1.000000000000000000, -0.000000000000000000 ) ) ;
#12433 = CARTESIAN_POINT ( 'NONE',  ( -3.511755186886851288, 2.826662030176404716, -3.597382984111576754 ) ) ;
#12434 = DIRECTION ( 'NONE',  ( -1.733449886265891589E-32, 4.190823558986610327E-31, -1.000000000000000000 ) ) ;
#12435 = CARTESIAN_POINT ( 'NONE',  ( 37.48161866288229760, 10.82270004028423571, -10.09721192197979711 ) ) ;
#12436 = DIRECTION ( 'NONE',  ( 5.551115123125782702E-16, 1.201780285297635172E-31, -1.000000000000000000 ) ) ;
#12437 = DIRECTION ( 'NONE',  ( -1.733449886265891589E-32, 4.190823558986610327E-31, -1.000000000000000000 ) ) ;
#12438 = LINE ( 'NONE', #17985, #3983 ) ;
#12439 = FACE_OUTER_BOUND ( 'NONE', #19575, .T. ) ;
#12441 = CIRCLE ( 'NONE', #14330, 6.000000000000022204 ) ;
#12440 = CARTESIAN_POINT ( 'NONE',  ( 7.596194078004423034, 47.59619407671642222, -26.00000000000000000 ) ) ;
#12442 = AXIS2_PLACEMENT_3D ( 'NONE', #1393, #22929, #12195 ) ;
#12443 = VERTEX_POINT ( 'NONE', #2767 ) ;
#12444 = ITEM_DEFINED_TRANSFORMATION ( 'NONE', 'NONE', #22534,  #22115 ) ;
#12445 = ORIENTED_EDGE ( 'NONE', *, *, #7785, .T. ) ;
#12446 = CARTESIAN_POINT ( 'NONE',  ( -6.525563119727650907, 36.00216957434302856, -26.37497832018746280 ) ) ;
#12448 = ORIENTED_EDGE ( 'NONE', *, *, #16709, .T. ) ;
#12447 = EDGE_LOOP ( 'NONE', ( #1127, #7399, #4421, #4721, #16084, #16112, #11611 ) ) ;
#12449 = CARTESIAN_POINT ( 'NONE',  ( -3.649122391096772500, -1.701165921963347705, -3.179534615582980894 ) ) ;
#12450 = LINE ( 'NONE', #17635, #17096 ) ;
#12451 = CARTESIAN_POINT ( 'NONE',  ( 1.848892746611746769E-30, 8.456305733849119291E-32, 2.500000000000003997 ) ) ;
#12452 = CARTESIAN_POINT ( 'NONE',  ( 0.000000000000000000, 3.031088913245536087, 1.749999999999998002 ) ) ;
#12453 = EDGE_LOOP ( 'NONE', ( #19701, #8961, #22471, #21286, #9363, #16083 ) ) ;
#12454 = CYLINDRICAL_SURFACE ( 'NONE', #8018, 0.5000000000000000000 ) ;
#12455 = CONICAL_SURFACE ( 'NONE', #5332, 7.500000000000001776, 1.308996938995750092 ) ;
#12456 = CIRCLE ( 'NONE', #3082, 2.800000000000017586 ) ;
#12457 = DIRECTION ( 'NONE',  ( -1.000000000000000000, 1.276756478318923119E-15, -1.387778780781436998E-15 ) ) ;
#12458 = DIRECTION ( 'NONE',  ( 1.000000000000000000, 0.000000000000000000, 0.000000000000000000 ) ) ;
#12459 = EDGE_CURVE ( 'NONE', #10770, #17530, #2649, .T. ) ;
#12460 = CARTESIAN_POINT ( 'NONE',  ( -7.332081355611494544, -13.77321347121581319, 7.890992604157061052 ) ) ;
#12461 = FACE_OUTER_BOUND ( 'NONE', #9068, .T. ) ;
#12462 = DIRECTION ( 'NONE',  ( 2.013525853228518840E-32, -6.902532920683810383E-31, 1.000000000000000000 ) ) ;
#12463 = DIRECTION ( 'NONE',  ( -1.000000000000000000, -4.440892098500626162E-16, 5.551115123125782702E-16 ) ) ;
#12464 = LINE ( 'NONE', #17646, #15327 ) ;
#12465 = CARTESIAN_POINT ( 'NONE',  ( -55.05572809000125289, 3.200000000000022382, -10.00000000000006395 ) ) ;
#12466 = FACE_OUTER_BOUND ( 'NONE', #983, .T. ) ;
#12467 = ORIENTED_EDGE ( 'NONE', *, *, #11241, .F. ) ;
#12468 = CARTESIAN_POINT ( 'NONE',  ( -83.51225780769253504, 17.65948356667608365, 25.91570243528392226 ) ) ;
#12469 = AXIS2_PLACEMENT_3D ( 'NONE', #18448, #9862, #7633 ) ;
#12471 = EDGE_LOOP ( 'NONE', ( #9129, #2445, #20415 ) ) ;
#12470 = ORIENTED_EDGE ( 'NONE', *, *, #15156, .T. ) ;
#12472 = ORIENTED_EDGE ( 'NONE', *, *, #19933, .F. ) ;
#12474 = ORIENTED_EDGE ( 'NONE', *, *, #9226, .T. ) ;
#12473 = EDGE_LOOP ( 'NONE', ( #1720, #9787, #21369, #16260, #3430, #13094, #23020 ) ) ;
#12475 = CARTESIAN_POINT ( 'NONE',  ( 2.742827927723032300, 3.035229711105330352, -3.433252694550416706 ) ) ;
#12476 = CARTESIAN_POINT ( 'NONE',  ( -3.999999999708139686, 49.99999999900385461, -18.99999999999998934 ) ) ;
#12477 = DIRECTION ( 'NONE',  ( 0.9706398123736370565, 1.133987551255197639E-30, 0.2405376366294281198 ) ) ;
#12478 = LINE ( 'NONE', #23101, #13952 ) ;
#12479 = CIRCLE ( 'NONE', #13229, 2.550000000000002043 ) ;
#12480 = CARTESIAN_POINT ( 'NONE',  ( 37.00000000000017053, 0.000000000000000000, -6.499999999999964473 ) ) ;
#12481 = CARTESIAN_POINT ( 'NONE',  ( -8.160037397871438003, -0.008793114504473772963, 6.662331851011921380 ) ) ;
#12482 = LINE ( 'NONE', #7210, #5754 ) ;
#12483 = CARTESIAN_POINT ( 'NONE',  ( 2.775557561562891351E-14, 11.99999999999999645, 6.938893903907228378E-15 ) ) ;
#12484 = CARTESIAN_POINT ( 'NONE',  ( 4.071447262713891568, -4.041451884327432076, 1.040834085586084257E-14 ) ) ;
#12485 = CARTESIAN_POINT ( 'NONE',  ( -6.938893903907228378E-14, -4.618802153517020059, -0.3572655899081733644 ) ) ;
#12486 = VECTOR ( 'NONE', #9460, 1000.000000000000000 ) ;
#12487 = DIRECTION ( 'NONE',  ( 1.733449886265890494E-32, 4.190823558986611203E-31, -1.000000000000000000 ) ) ;
#12488 = AXIS2_PLACEMENT_3D ( 'NONE', #12777, #2299, #19960 ) ;
#12489 = CARTESIAN_POINT ( 'NONE',  ( 26.45000000029184051, 16.99999999900385461, -19.49999999999998934 ) ) ;
#12490 = AXIS2_PLACEMENT_3D ( 'NONE', #16043, #21372, #1820 ) ;
#12491 = AXIS2_PLACEMENT_3D ( 'NONE', #18501, #5924, #16949 ) ;
#12492 = PRODUCT_RELATED_PRODUCT_CATEGORY ( 'part', '', ( #13999 ) ) ;
#12493 = DIRECTION ( 'NONE',  ( 0.000000000000000000, 0.000000000000000000, -1.000000000000000000 ) ) ;
#12494 = CARTESIAN_POINT ( 'NONE',  ( -12.84999999999998721, -12.50000000000002842, 5.750000000000060396 ) ) ;
#12495 = CARTESIAN_POINT ( 'NONE',  ( -2.500000000000002220, 0.000000000000000000, -5.574599999999999334 ) ) ;
#12496 = FACE_OUTER_BOUND ( 'NONE', #2794, .T. ) ;
#12497 = EDGE_LOOP ( 'NONE', ( #19568, #3916, #3585, #9185 ) ) ;
#12498 = EDGE_CURVE ( 'NONE', #3520, #84, #14066, .T. ) ;
#12500 = ORIENTED_EDGE ( 'NONE', *, *, #5927, .F. ) ;
#12499 = ORIENTED_EDGE ( 'NONE', *, *, #1356, .T. ) ;
#12501 = VERTEX_POINT ( 'NONE', #10059 ) ;
#12502 = CIRCLE ( 'NONE', #22664, 0.5000000000000018874 ) ;
#12503 = TOROIDAL_SURFACE ( 'NONE', #7682, 6.000000000000000000, 0.5000000000000000000 ) ;
#12504 =( BOUNDED_CURVE ( )  B_SPLINE_CURVE ( 3, ( #17769, #1658, #7081, #9760 ),
 .UNSPECIFIED., .F., .F. ) 
 B_SPLINE_CURVE_WITH_KNOTS ( ( 4, 4 ),
 ( 1.570796326794896558, 2.617993877991505514 ),
 .UNSPECIFIED. ) 
 CURVE ( )  GEOMETRIC_REPRESENTATION_ITEM ( )  RATIONAL_B_SPLINE_CURVE ( ( 1.000000000000000000, 0.9106836025229571030, 0.9106836025229571030, 1.000000000000000000 ) ) 
 REPRESENTATION_ITEM ( '' )  );
#12506 = ORIENTED_EDGE ( 'NONE', *, *, #16907, .F. ) ;
#12505 = ORIENTED_EDGE ( 'NONE', *, *, #1632, .F. ) ;
#12507 = B_SPLINE_CURVE_WITH_KNOTS ( 'NONE', 3,
 ( #1142, #8432, #19474, #8770 ),
 .UNSPECIFIED., .F., .F.,
 ( 4, 4 ),
 ( 0.000000000000000000, 1.361771040845327923E-05 ),
 .UNSPECIFIED. ) ;
#12508 = CIRCLE ( 'NONE', #2733, 0.2500000000000002220 ) ;
#12509 = VERTEX_POINT ( 'NONE', #13480 ) ;
#12510 = CIRCLE ( 'NONE', #3855, 0.4999999999999984457 ) ;
#12511 = ORIENTED_EDGE ( 'NONE', *, *, #19579, .T. ) ;
#12512 = VERTEX_POINT ( 'NONE', #4527 ) ;
#12513 = DIRECTION ( 'NONE',  ( 2.013525853228507892E-32, 6.902532920683810383E-31, -1.000000000000000000 ) ) ;
#12514 = LINE ( 'NONE', #16154, #8756 ) ;
#12515 = DIRECTION ( 'NONE',  ( -1.445602896647339163E-16, 1.000000000000000000, 0.000000000000000000 ) ) ;
#12516 = DIRECTION ( 'NONE',  ( 1.550910762415566494E-16, 1.000000000000000000, -8.135128085091684243E-31 ) ) ;
#12517 = DIRECTION ( 'NONE',  ( -0.000000000000000000, -0.000000000000000000, 1.000000000000000000 ) ) ;
#12518 = CARTESIAN_POINT ( 'NONE',  ( -2.742413778650615086, 1.750000000000001554, -4.750000000000004441 ) ) ;
#12519 = CARTESIAN_POINT ( 'NONE',  ( 66.26395429947832838, -7.000000000000006217, 6.000000000000172307 ) ) ;
#12520 = EDGE_CURVE ( 'NONE', #15489, #6825, #9939, .T. ) ;
#12521 = CARTESIAN_POINT ( 'NONE',  ( 2.775557561562891351E-14, 11.99999999999999645, 6.938893903907228378E-15 ) ) ;
#12522 = FACE_OUTER_BOUND ( 'NONE', #14056, .T. ) ;
#12523 = VECTOR ( 'NONE', #16421, 1000.000000000000000 ) ;
#12524 = VECTOR ( 'NONE', #22108, 1000.000000000000000 ) ;
#12525 = CARTESIAN_POINT ( 'NONE',  ( -6.230270079314315979, 13.95903802731504584, -16.98373150477994287 ) ) ;
#12526 = CARTESIAN_POINT ( 'NONE',  ( -7.884991313526885648, -1.682691736113209213, 7.773664271103597478 ) ) ;
#12527 = VECTOR ( 'NONE', #10779, 1000.000000000000000 ) ;
#12528 = ORIENTED_EDGE ( 'NONE', *, *, #11086, .T. ) ;
#12530 = EDGE_CURVE ( 'NONE', #11557, #20666, #5819, .T. ) ;
#12529 = AXIS2_PLACEMENT_3D ( 'NONE', #21182, #17876, #19284 ) ;
#12531 = TOROIDAL_SURFACE ( 'NONE', #9151, 6.500000000000005329, 0.5000000000000000000 ) ;
#12532 =( LENGTH_UNIT ( ) NAMED_UNIT ( * ) SI_UNIT ( .MILLI., .METRE. ) );
#12533 = DIRECTION ( 'NONE',  ( 0.5150787536377134934, 0.000000000000000000, 0.8571428571428567622 ) ) ;
#12534 = DIRECTION ( 'NONE',  ( -1.550910762415566494E-16, -1.000000000000000000, 8.135128085091684243E-31 ) ) ;
#12536 = EDGE_LOOP ( 'NONE', ( #1666, #14399, #6266, #8581, #12626, #17333 ) ) ;
#12535 = EDGE_LOOP ( 'NONE', ( #23261, #22609, #9042, #6095 ) ) ;
#12537 = EDGE_CURVE ( 'NONE', #8293, #16898, #20451, .T. ) ;
#12538 = ORIENTED_EDGE ( 'NONE', *, *, #1742, .F. ) ;
#12539 = EDGE_CURVE ( 'NONE', #18554, #6591, #3912, .T. ) ;
#12540 = EDGE_LOOP ( 'NONE', ( #11692, #19282, #11401, #18389, #10516, #23090 ) ) ;
#12541 = VERTEX_POINT ( 'NONE', #15109 ) ;
#12542 = LINE ( 'NONE', #21394, #18545 ) ;
#12543 = TOROIDAL_SURFACE ( 'NONE', #14044, 4.500000000000000888, 0.5000000000000000000 ) ;
#12544 = AXIS2_PLACEMENT_3D ( 'NONE', #15086, #22051, #2284 ) ;
#12545 = CARTESIAN_POINT ( 'NONE',  ( 7.909386411297023578, -0.6370970679665967085, 7.731447622712498635 ) ) ;
#12546 = VECTOR ( 'NONE', #20664, 1000.000000000000000 ) ;
#12547 = FACE_OUTER_BOUND ( 'NONE', #21614, .T. ) ;
#12548 = CARTESIAN_POINT ( 'NONE',  ( 4.050536630291712292, -3.778525289263205078, -0.5912575323400444116 ) ) ;
#12549 = DIRECTION ( 'NONE',  ( 0.6819983600625055820, 0.7313537016191637985, 4.996142016973858765E-16 ) ) ;
#12550 = FACE_BOUND ( 'NONE', #16397, .T. ) ;
#12551 = DIRECTION ( 'NONE',  ( 1.000000000000000000, 6.224605580259554159E-31, -2.887593071917436153E-31 ) ) ;
#12552 = DIRECTION ( 'NONE',  ( -1.000000000000000000, -1.424116703980846297E-16, 1.095779650622964657E-32 ) ) ;
#12553 = EDGE_CURVE ( 'NONE', #12207, #14170, #21218, .T. ) ;
#12554 = ADVANCED_FACE ( 'NONE', ( #4869 ), #930, .T. ) ;
#12555 = LINE ( 'NONE', #21406, #12968 ) ;
#12556 = EDGE_CURVE ( 'NONE', #14050, #19728, #18953, .T. ) ;
#12557 = DIRECTION ( 'NONE',  ( 0.000000000000000000, 0.000000000000000000, -1.000000000000000000 ) ) ;
#12558 = CARTESIAN_POINT ( 'NONE',  ( 0.000000000000000000, 1.750000000000001554, 0.000000000000000000 ) ) ;
#12559 = CARTESIAN_POINT ( 'NONE',  ( -55.25320565519145788, -0.5000000000000281997, 10.00000000000009237 ) ) ;
#12560 = AXIS2_PLACEMENT_3D ( 'NONE', #10608, #1897, #17802 ) ;
#12561 = PLANE ( 'NONE',  #22117 ) ;
#12562 = CIRCLE ( 'NONE', #1670, 0.5000000000000004441 ) ;
#12563 = AXIS2_PLACEMENT_3D ( 'NONE', #6257, #6602, #13776 ) ;
#12564 = DIRECTION ( 'NONE',  ( 1.454462294001240516E-30, 1.000000000000000000, 0.000000000000000000 ) ) ;
#12565 = VERTEX_POINT ( 'NONE', #7133 ) ;
#12566 = ADVANCED_FACE ( 'NONE', ( #6643 ), #15799, .F. ) ;
#12567 = AXIS2_PLACEMENT_3D ( 'NONE', #15076, #10033, #8275 ) ;
#12568 = ADVANCED_FACE ( 'NONE', ( #10521 ), #8877, .T. ) ;
#12569 = ORIENTED_EDGE ( 'NONE', *, *, #10947, .T. ) ;
#12570 = ADVANCED_FACE ( 'NONE', ( #7009 ), #21245, .F. ) ;
#12571 = CARTESIAN_POINT ( 'NONE',  ( -4.720100440588442581, 36.44386358680064575, -26.00000000000000000 ) ) ;
#12572 = ORIENTED_EDGE ( 'NONE', *, *, #3481, .F. ) ;
#12573 = DIRECTION ( 'NONE',  ( 1.133987551255203069E-30, -2.220446049250310616E-16, 1.000000000000000000 ) ) ;
#12574 = CARTESIAN_POINT ( 'NONE',  ( 30.00000000029184832, 2.999999999003851503, -45.00000000000000000 ) ) ;
#12575 = CARTESIAN_POINT ( 'NONE',  ( 4.052424581287677796, -3.786734753435081480, -0.5771415817958118755 ) ) ;
#12576 = FACE_OUTER_BOUND ( 'NONE', #21442, .T. ) ;
#12577 = MECHANICAL_DESIGN_GEOMETRIC_PRESENTATION_REPRESENTATION (  '', ( #4302 ), #7701 ) ;
#12578 = ORIENTED_EDGE ( 'NONE', *, *, #11079, .F. ) ;
#12579 = TOROIDAL_SURFACE ( 'NONE', #2436, 3.500000000000001776, 0.5000000000000000000 ) ;
#12580 = DIRECTION ( 'NONE',  ( 3.885780586188016830E-16, 4.437342591868156373E-31, -1.000000000000000000 ) ) ;
#12581 = CARTESIAN_POINT ( 'NONE',  ( -0.9238745060512592033, -1.710161125114598946, -4.750000000000025757 ) ) ;
#12582 = CARTESIAN_POINT ( 'NONE',  ( -6.999999999708142795, 13.99999999900385106, -26.00000000000000000 ) ) ;
#12583 = CARTESIAN_POINT ( 'NONE',  ( 42.50000000000014921, 8.500000000000003553, -12.49999999999998401 ) ) ;
#12584 = CARTESIAN_POINT ( 'NONE',  ( -55.25320565519145788, -2.775557561562891351E-14, 10.00000000000009237 ) ) ;
#12585 = DIRECTION ( 'NONE',  ( 2.013525853228507892E-32, 6.902532920683810383E-31, -1.000000000000000000 ) ) ;
#12586 = CARTESIAN_POINT ( 'NONE',  ( 4.165266963751722784, 2.049631966912018211, -3.550066703508910848 ) ) ;
#12587 = CARTESIAN_POINT ( 'NONE',  ( 3.950241966887848122, -3.393956070637773603, 1.121495646999037143 ) ) ;
#12588 = DIRECTION ( 'NONE',  ( 3.885780586188016830E-16, 4.437342591868156373E-31, -1.000000000000000000 ) ) ;
#12589 = ORIENTED_EDGE ( 'NONE', *, *, #14098, .T. ) ;
#12590 = AXIS2_PLACEMENT_3D ( 'NONE', #3400, #12072, #5662 ) ;
#12591 = APPLICATION_PROTOCOL_DEFINITION ( 'draft international standard', 'automotive_design', 1998, #4265 ) ;
#12592 = EDGE_CURVE ( 'NONE', #22558, #9917, #22705, .T. ) ;
#12593 = VECTOR ( 'NONE', #2587, 1000.000000000000000 ) ;
#12595 = ORIENTED_EDGE ( 'NONE', *, *, #4040, .T. ) ;
#12594 = ORIENTED_EDGE ( 'NONE', *, *, #17713, .F. ) ;
#12596 = ADVANCED_FACE ( 'NONE', ( #14292 ), #17689, .T. ) ;
#12597 = ORIENTED_EDGE ( 'NONE', *, *, #1907, .F. ) ;
#12599 = EDGE_LOOP ( 'NONE', ( #4395, #22816, #19489, #21085 ) ) ;
#12598 = EDGE_LOOP ( 'NONE', ( #8554, #5828, #17991, #1668 ) ) ;
#12600 = CARTESIAN_POINT ( 'NONE',  ( 0.5449313310646434205, 4.304185902837014410, -3.316620875263985191 ) ) ;
#12601 = CARTESIAN_POINT ( 'NONE',  ( 0.000000000000000000, 0.000000000000000000, 0.000000000000000000 ) ) ;
#12602 = CARTESIAN_POINT ( 'NONE',  ( 7.725871784772684769, -12.18565941508499861, 8.100883686805255834 ) ) ;
#12603 = AXIS2_PLACEMENT_3D ( 'NONE', #17729, #5150, #12314 ) ;
#12604 = FACE_OUTER_BOUND ( 'NONE', #2175, .T. ) ;
#12605 = DIRECTION ( 'NONE',  ( -9.693457064947022734E-26, 0.000000000000000000, 1.000000000000000000 ) ) ;
#12606 = CARTESIAN_POINT ( 'NONE',  ( 2.775557561562891351E-14, 11.99999999999999645, 6.938893903907228378E-15 ) ) ;
#12607 = CARTESIAN_POINT ( 'NONE',  ( 108.2426266706971205, -13.02760560296367665, -6.500000000000075495 ) ) ;
#12608 = DIRECTION ( 'NONE',  ( -2.172745813409349776E-17, 1.000000000000000000, -1.309377075419428048E-16 ) ) ;
#12609 = DIRECTION ( 'NONE',  ( -2.775557561562902444E-17, 0.000000000000000000, -1.000000000000000000 ) ) ;
#12610 = DIRECTION ( 'NONE',  ( 1.000000000000000000, 1.910522504832140594E-31, -5.551115123125818447E-17 ) ) ;
#12611 = LINE ( 'NONE', #16134, #6310 ) ;
#12612 = AXIS2_PLACEMENT_3D ( 'NONE', #5321, #21565, #12722 ) ;
#12613 = CARTESIAN_POINT ( 'NONE',  ( 12.84999999999997300, -14.00000000000007105, 5.551115123125782702E-14 ) ) ;
#12614 = DIRECTION ( 'NONE',  ( -1.000000000000000000, 0.000000000000000000, -0.000000000000000000 ) ) ;
#12615 = CARTESIAN_POINT ( 'NONE',  ( 7.856071383949647213, -0.04768060911160624388, 7.015054140272313887 ) ) ;
#12616 = ORIENTED_EDGE ( 'NONE', *, *, #15615, .F. ) ;
#12617 =( GEOMETRIC_REPRESENTATION_CONTEXT ( 3 ) GLOBAL_UNCERTAINTY_ASSIGNED_CONTEXT ( ( #8378 ) ) GLOBAL_UNIT_ASSIGNED_CONTEXT ( ( #9637, #6116, #11866 ) ) REPRESENTATION_CONTEXT ( 'NONE', 'WORKASPACE' ) );
#12618 = SURFACE_STYLE_USAGE ( .BOTH. , #21583 ) ;
#12620 = EDGE_LOOP ( 'NONE', ( #11694, #17338, #18496 ) ) ;
#12619 = EDGE_LOOP ( 'NONE', ( #21112, #4729, #7174, #2325, #22853, #19631, #7594 ) ) ;
#12621 = UNCERTAINTY_MEASURE_WITH_UNIT (LENGTH_MEASURE( 1.000000000000000082E-05 ), #22203, 'distance_accuracy_value', 'NONE');
#12622 = ORIENTED_EDGE ( 'NONE', *, *, #4619, .T. ) ;
#12624 = ORIENTED_EDGE ( 'NONE', *, *, #13280, .T. ) ;
#12623 = ORIENTED_EDGE ( 'NONE', *, *, #17112, .T. ) ;
#12625 = CIRCLE ( 'NONE', #7740, 4.499999999999988454 ) ;
#12626 = ORIENTED_EDGE ( 'NONE', *, *, #22669, .T. ) ;
#12627 = ORIENTED_EDGE ( 'NONE', *, *, #9230, .F. ) ;
#12628 = ORIENTED_EDGE ( 'NONE', *, *, #19414, .T. ) ;
#12629 = DIRECTION ( 'NONE',  ( -1.000000000000000000, 1.424116703980815236E-16, 2.931272055834072749E-32 ) ) ;
#12630 = VECTOR ( 'NONE', #10693, 1000.000000000000000 ) ;
#12631 = CARTESIAN_POINT ( 'NONE',  ( 119.5756419024615838, -6.500000000000061284, -6.499999999999992006 ) ) ;
#12632 = LINE ( 'NONE', #16384, #5640 ) ;
#12633 = CARTESIAN_POINT ( 'NONE',  ( -6.999999999999992006, -2.645898033750305522, 9.250000000000021316 ) ) ;
#12634 = EDGE_CURVE ( 'NONE', #20007, #2500, #556, .T. ) ;
#12635 = DIRECTION ( 'NONE',  ( 0.000000000000000000, 0.000000000000000000, 1.000000000000000000 ) ) ;
#12636 = CARTESIAN_POINT ( 'NONE',  ( -42.54314575050785407, -4.000000000000021316, 8.000000000000007105 ) ) ;
#12637 = CARTESIAN_POINT ( 'NONE',  ( -0.5636800770137567751, -4.293361309318373564, -3.531542292954506390 ) ) ;
#12638 =( NAMED_UNIT ( * ) PLANE_ANGLE_UNIT ( ) SI_UNIT ( $, .RADIAN. ) );
#12639 = CARTESIAN_POINT ( 'NONE',  ( 2.775557561562891351E-14, 0.000000000000000000, -6.499999999999950262 ) ) ;
#12640 = LINE ( 'NONE', #4353, #10683 ) ;
#12641 = CARTESIAN_POINT ( 'NONE',  ( -6.999999999708142795, 38.99999999900385461, -22.50000000000000000 ) ) ;
#12642 = ORIENTED_EDGE ( 'NONE', *, *, #23227, .F. ) ;
#12643 = UNCERTAINTY_MEASURE_WITH_UNIT (LENGTH_MEASURE( 1.000000000000000082E-05 ), #8412, 'distance_accuracy_value', 'NONE');
#12644 = AXIS2_PLACEMENT_3D ( 'NONE', #3160, #3497, #10669 ) ;
#12645 = B_SPLINE_CURVE_WITH_KNOTS ( 'NONE', 3,
 ( #4329, #2232, #21999, #16453, #18689, #13291, #13175, #364 ),
 .UNSPECIFIED., .F., .F.,
 ( 4, 2, 2, 4 ),
 ( 2.465131517408427001E-07, 0.001183067374689895750, 0.001774477805458973606, 0.002365888236228051462 ),
 .UNSPECIFIED. ) ;
#12646 = LINE ( 'NONE', #17598, #19498 ) ;
#12648 = ORIENTED_EDGE ( 'NONE', *, *, #9405, .F. ) ;
#12647 = VERTEX_POINT ( 'NONE', #1577 ) ;
#12649 = VECTOR ( 'NONE', #13227, 1000.000000000000000 ) ;
#12650 = EDGE_LOOP ( 'NONE', ( #12467, #19956 ) ) ;
#12651 = VERTEX_POINT ( 'NONE', #10287 ) ;
#12652 = VECTOR ( 'NONE', #7333, 1000.000000000000000 ) ;
#12653 = ORIENTED_EDGE ( 'NONE', *, *, #4894, .T. ) ;
#12654 = ORIENTED_EDGE ( 'NONE', *, *, #1787, .T. ) ;
#12655 = DIRECTION ( 'NONE',  ( -1.454462294001240516E-30, -1.000000000000000000, 0.000000000000000000 ) ) ;
#12656 = CARTESIAN_POINT ( 'NONE',  ( 4.175813232069149450, 2.061359961916364725, -3.570380186727398986 ) ) ;
#12657 = CARTESIAN_POINT ( 'NONE',  ( 4.180345304246191773, 2.049116244671347786, -3.591763845239305919 ) ) ;
#12658 = FACE_OUTER_BOUND ( 'NONE', #16636, .T. ) ;
#12659 = EDGE_CURVE ( 'NONE', #16028, #4291, #5350, .T. ) ;
#12660 = FACE_OUTER_BOUND ( 'NONE', #19980, .T. ) ;
#12661 = CARTESIAN_POINT ( 'NONE',  ( 42.50000000000014921, 2.999999999999999112, 2.000000000000071054 ) ) ;
#12662 = DIRECTION ( 'NONE',  ( 8.438582421954109416E-32, 0.000000000000000000, 1.000000000000000000 ) ) ;
#12663 = DIRECTION ( 'NONE',  ( -1.550910762415566494E-16, -1.000000000000000000, 8.135128085091684243E-31 ) ) ;
#12664 = VECTOR ( 'NONE', #12534, 1000.000000000000000 ) ;
#12665 = CARTESIAN_POINT ( 'NONE',  ( -7.162073728446612719, -2.365283217609512434, 7.945145523438274182 ) ) ;
#12666 = CARTESIAN_POINT ( 'NONE',  ( 85.68838070902457105, -9.818697260249752645, -6.500000000000019540 ) ) ;
#12667 = VECTOR ( 'NONE', #23085, 1000.000000000000000 ) ;
#12668 = ADVANCED_FACE ( 'NONE', ( #5111 ), #22766, .T. ) ;
#12669 = EDGE_CURVE ( 'NONE', #1999, #10307, #6551, .T. ) ;
#12670 = B_SPLINE_CURVE_WITH_KNOTS ( 'NONE', 3,
 ( #664, #18649, #9828, #1134, #6306, #4403, #8299, #15457, #900, #7833, #15347, #6422, #11695, #8062, #20889, #13593 ),
 .UNSPECIFIED., .F., .F.,
 ( 4, 3, 3, 3, 3, 4 ),
 ( 0.000000000000000000, 3.315506744709602110E-05, 6.608280158699779622E-05, 0.0001026520855291460272, 0.0001376952025664770357, 0.0001398064759190588782 ),
 .UNSPECIFIED. ) ;
#12671 = DIRECTION ( 'NONE',  ( 0.000000000000000000, 0.000000000000000000, 1.000000000000000000 ) ) ;
#12672 = CARTESIAN_POINT ( 'NONE',  ( 12.84999999999998721, -1.500000000000004885, -5.749999999999976907 ) ) ;
#12674 = EDGE_CURVE ( 'NONE', #17239, #9471, #2407, .T. ) ;
#12673 = CARTESIAN_POINT ( 'NONE',  ( -7.216878364870350282, 4.999999999999984901, 2.499999999999995115 ) ) ;
#12675 = AXIS2_PLACEMENT_3D ( 'NONE', #17674, #14158, #1346 ) ;
#12676 = DIRECTION ( 'NONE',  ( 1.066786462891689527E-26, 6.656013887802287108E-31, 1.000000000000000000 ) ) ;
#12677 = LINE ( 'NONE', #15965, #19432 ) ;
#12678 = ORIENTED_EDGE ( 'NONE', *, *, #13859, .F. ) ;
#12679 = AXIS2_PLACEMENT_3D ( 'NONE', #4972, #12253, #8625 ) ;
#12680 = VERTEX_POINT ( 'NONE', #1465 ) ;
#12681 = AXIS2_PLACEMENT_3D ( 'NONE', #14811, #2338, #16787 ) ;
#12682 = CIRCLE ( 'NONE', #11555, 3.499999999999999556 ) ;
#12683 = CARTESIAN_POINT ( 'NONE',  ( -65.55642023346354108, 2.700000000000056577, -11.87813525200309783 ) ) ;
#12684 = ADVANCED_FACE ( 'NONE', ( #19224 ), #19705, .F. ) ;
#12685 = EDGE_CURVE ( 'NONE', #1665, #8753, #8760, .T. ) ;
#12686 = ORIENTED_EDGE ( 'NONE', *, *, #5389, .F. ) ;
#12688 = CIRCLE ( 'NONE', #1794, 0.5000000000000029976 ) ;
#12687 = APPLICATION_CONTEXT ( 'automotive_design' ) ;
#12689 = CARTESIAN_POINT ( 'NONE',  ( 88.75737332930587797, -10.52760560296347947, 6.500000000000075495 ) ) ;
#12690 = DIRECTION ( 'NONE',  ( 1.000000000000000000, 0.000000000000000000, 0.000000000000000000 ) ) ;
#12691 = CARTESIAN_POINT ( 'NONE',  ( 6.999999999999978684, -10.98142396999974757, 8.916666666666712260 ) ) ;
#12692 = DIRECTION ( 'NONE',  ( 1.939787525279694947E-32, -6.902532920683810383E-31, 1.000000000000000000 ) ) ;
#12693 = AXIS2_PLACEMENT_3D ( 'NONE', #8744, #15903, #23114 ) ;
#12694 = ORIENTED_EDGE ( 'NONE', *, *, #13293, .F. ) ;
#12695 = DIRECTION ( 'NONE',  ( 0.000000000000000000, 0.000000000000000000, 1.000000000000000000 ) ) ;
#12696 = CARTESIAN_POINT ( 'NONE',  ( 2.775557561562891351E-14, 3.000000000000006217, -6.499999999999950262 ) ) ;
#12697 = CIRCLE ( 'NONE', #19096, 0.5000000000000029976 ) ;
#12698 = ADVANCED_FACE ( 'NONE', ( #10171 ), #17334, .T. ) ;
#12699 = CARTESIAN_POINT ( 'NONE',  ( -5.484827557301452217, 1.749999999999973799, -2.775557561562891351E-14 ) ) ;
#12700 = CARTESIAN_POINT ( 'NONE',  ( -90.55603112840523750, -6.245004513516505540E-14, -7.432974388601742533 ) ) ;
#12701 = CARTESIAN_POINT ( 'NONE',  ( -5.484827557301452217, 1.749999999999973799, -2.775557561562891351E-14 ) ) ;
#12702 = CYLINDRICAL_SURFACE ( 'NONE', #16412, 0.4999999999999995559 ) ;
#12703 = EDGE_CURVE ( 'NONE', #6879, #2848, #5470, .T. ) ;
#12704 = CARTESIAN_POINT ( 'NONE',  ( 4.175326769692856210, 2.060699556488918560, -3.569236330973474924 ) ) ;
#12705 = DIRECTION ( 'NONE',  ( -1.000000000000000000, 0.000000000000000000, 0.000000000000000000 ) ) ;
#12707 = EDGE_CURVE ( 'NONE', #7514, #1104, #7351, .T. ) ;
#12706 = FILL_AREA_STYLE ('',( #5187 ) ) ;
#12708 =( GEOMETRIC_REPRESENTATION_CONTEXT ( 3 ) GLOBAL_UNCERTAINTY_ASSIGNED_CONTEXT ( ( #18049 ) ) GLOBAL_UNIT_ASSIGNED_CONTEXT ( ( #441, #9615, #7193 ) ) REPRESENTATION_CONTEXT ( 'NONE', 'WORKASPACE' ) );
#12709 = CARTESIAN_POINT ( 'NONE',  ( 54.42435809754115894, 2.499999999999946709, -5.999999999999950262 ) ) ;
#12710 = ORIENTED_EDGE ( 'NONE', *, *, #3258, .F. ) ;
#12711 = CIRCLE ( 'NONE', #4423, 0.4999999999999995559 ) ;
#12712 = APPLICATION_PROTOCOL_DEFINITION ( 'draft international standard', 'automotive_design', 1998, #11175 ) ;
#12714 = ORIENTED_EDGE ( 'NONE', *, *, #4052, .T. ) ;
#12713 = ORIENTED_EDGE ( 'NONE', *, *, #23022, .T. ) ;
#12715 = ORIENTED_EDGE ( 'NONE', *, *, #11127, .T. ) ;
#12716 = EDGE_CURVE ( 'NONE', #6413, #12275, #7696, .T. ) ;
#12718 = ORIENTED_EDGE ( 'NONE', *, *, #18193, .T. ) ;
#12717 = ORIENTED_EDGE ( 'NONE', *, *, #7491, .T. ) ;
#12719 = CARTESIAN_POINT ( 'NONE',  ( 1.390230914382568406, 4.043987460488565944, -3.502507215260532547 ) ) ;
#12720 = CARTESIAN_POINT ( 'NONE',  ( 8.697224362267983011, 0.000000000000000000, 6.249999999999977796 ) ) ;
#12721 = CARTESIAN_POINT ( 'NONE',  ( 7.161440864725792999, -11.61224748569070009, 7.973376427817330914 ) ) ;
#12722 = DIRECTION ( 'NONE',  ( -1.000000000000000000, 1.511687600494058571E-14, -3.717264591378832268E-16 ) ) ;
#12723 = EDGE_CURVE ( 'NONE', #2067, #19898, #16290, .T. ) ;
#12724 = CARTESIAN_POINT ( 'NONE',  ( 2.499999999999998668, 2.000000000000001776, -18.75000000000001066 ) ) ;
#12725 = CARTESIAN_POINT ( 'NONE',  ( -43.46238456605043865, -4.919238815542549936, 7.500000000000062172 ) ) ;
#12726 = DIRECTION ( 'NONE',  ( 3.885780586188016830E-16, 4.437342591868156373E-31, -1.000000000000000000 ) ) ;
#12727 = AXIS2_PLACEMENT_3D ( 'NONE', #5403, #8925, #19512 ) ;
#12728 = CARTESIAN_POINT ( 'NONE',  ( -1.387778780781445676E-14, -24.99999999999998224, 0.000000000000000000 ) ) ;
#12729 = CONICAL_SURFACE ( 'NONE', #5236, 3.500000000000004441, 1.047197551196600296 ) ;
#12730 = CARTESIAN_POINT ( 'NONE',  ( 2.742413778650823364, 1.325747111984056037, -4.750000000000000888 ) ) ;
#12731 = CARTESIAN_POINT ( 'NONE',  ( 37.00000000000006395, 10.75000000000000000, -10.43301270189220276 ) ) ;
#12732 = CARTESIAN_POINT ( 'NONE',  ( 0.2499999999999655276, 2.000000000000015543, -2.000000000000001776 ) ) ;
#12733 = DIRECTION ( 'NONE',  ( -3.885780586188016830E-16, -4.437342591868156373E-31, 1.000000000000000000 ) ) ;
#12734 = DIRECTION ( 'NONE',  ( 0.000000000000000000, 0.000000000000000000, 1.000000000000000000 ) ) ;
#12735 = CARTESIAN_POINT ( 'NONE',  ( -6.590924991943732714, 35.99999999900384751, -18.75864816872293162 ) ) ;
#12736 = CARTESIAN_POINT ( 'NONE',  ( 7.500000000000008882, -0.9711575687493221309, 9.522727272727294690 ) ) ;
#12737 = ORIENTED_EDGE ( 'NONE', *, *, #11876, .T. ) ;
#12738 = SURFACE_SIDE_STYLE ('',( #16252 ) ) ;
#12740 = VERTEX_POINT ( 'NONE', #7576 ) ;
#12739 = VERTEX_POINT ( 'NONE', #1813 ) ;
#12741 = ORIENTED_EDGE ( 'NONE', *, *, #22197, .T. ) ;
#12742 = AXIS2_PLACEMENT_3D ( 'NONE', #18073, #8548, #23144 ) ;
#12744 = ORIENTED_EDGE ( 'NONE', *, *, #21171, .F. ) ;
#12743 = ORIENTED_EDGE ( 'NONE', *, *, #20305, .F. ) ;
#12745 = AXIS2_PLACEMENT_3D ( 'NONE', #18314, #2192, #21966 ) ;
#12746 = EDGE_LOOP ( 'NONE', ( #14202, #13033, #417, #13182 ) ) ;
#12747 = CARTESIAN_POINT ( 'NONE',  ( 4.175572532730925879, 2.061029303918053834, 3.569807470274390493 ) ) ;
#12748 = ORIENTED_EDGE ( 'NONE', *, *, #3551, .T. ) ;
#12749 = ORIENTED_EDGE ( 'NONE', *, *, #2867, .T. ) ;
#12750 = ADVANCED_FACE ( 'NONE', ( #21704 ), #2154, .F. ) ;
#12751 = DIRECTION ( 'NONE',  ( 2.013525853228507892E-32, 6.902532920683810383E-31, -1.000000000000000000 ) ) ;
#12752 = CIRCLE ( 'NONE', #6008, 4.749999999999986677 ) ;
#12753 = CARTESIAN_POINT ( 'NONE',  ( 88.75737332930597745, -13.02760560296348302, 6.500000000000103029 ) ) ;
#12754 = EDGE_CURVE ( 'NONE', #17189, #9711, #18793, .T. ) ;
#12755 = CARTESIAN_POINT ( 'NONE',  ( -45.56568542494964191, 2.108831175456939100, -8.000000000000062172 ) ) ;
#12756 =( GEOMETRIC_REPRESENTATION_CONTEXT ( 3 ) GLOBAL_UNCERTAINTY_ASSIGNED_CONTEXT ( ( #13117 ) ) GLOBAL_UNIT_ASSIGNED_CONTEXT ( ( #12030, #886, #9818 ) ) REPRESENTATION_CONTEXT ( 'NONE', 'WORKASPACE' ) );
#12757 = CARTESIAN_POINT ( 'NONE',  ( -90.55603112840530855, 3.200000000000057021, -7.432974388601742533 ) ) ;
#12758 = CARTESIAN_POINT ( 'NONE',  ( -45.01801948466087566, -6.474873734152949645, 7.500000000000089706 ) ) ;
#12759 = FACE_OUTER_BOUND ( 'NONE', #7368, .T. ) ;
#12760 = CARTESIAN_POINT ( 'NONE',  ( -3.472371940586150618, -2.614027278893177542, -3.320322319201808980 ) ) ;
#12761 = PRESENTATION_STYLE_ASSIGNMENT (( #21488 ) ) ;
#12762 = ADVANCED_FACE ( 'NONE', ( #7236 ), #10751, .F. ) ;
#12763 = CARTESIAN_POINT ( 'NONE',  ( 124.5000000000018332, -4.500000000000087041, -6.499999999999964473 ) ) ;
#12764 = DIRECTION ( 'NONE',  ( -2.168404344971017743E-16, -1.000000000000000000, 6.982962677686261977E-15 ) ) ;
#12765 = DIRECTION ( 'NONE',  ( 0.000000000000000000, 0.000000000000000000, -1.000000000000000000 ) ) ;
#12766 = ORIENTED_EDGE ( 'NONE', *, *, #14485, .F. ) ;
#12767 = DIRECTION ( 'NONE',  ( 2.220446049250313081E-16, -1.000000000000000000, 7.025792437124636392E-31 ) ) ;
#12768 = CIRCLE ( 'NONE', #15011, 10.00000000000006395 ) ;
#12770 = ORIENTED_EDGE ( 'NONE', *, *, #23149, .T. ) ;
#12769 = ORIENTED_EDGE ( 'NONE', *, *, #20475, .F. ) ;
#12771 = AXIS2_PLACEMENT_3D ( 'NONE', #15767, #17532, #4945 ) ;
#12772 = EDGE_CURVE ( 'NONE', #21928, #2848, #4035, .T. ) ;
#12773 = ORIENTED_EDGE ( 'NONE', *, *, #2040, .T. ) ;
#12774 = VERTEX_POINT ( 'NONE', #18060 ) ;
#12775 = VERTEX_POINT ( 'NONE', #22042 ) ;
#12776 = LINE ( 'NONE', #11344, #19677 ) ;
#12777 = CARTESIAN_POINT ( 'NONE',  ( 0.000000000000000000, 0.000000000000000000, -4.694516984716116781 ) ) ;
#12778 = CARTESIAN_POINT ( 'NONE',  ( 4.175326769692856210, -2.060699556488970074, -3.569236330973445170 ) ) ;
#12779 = CYLINDRICAL_SURFACE ( 'NONE', #21143, 2.550000000000010481 ) ;
#12780 = CARTESIAN_POINT ( 'NONE',  ( 6.495190528383244732, 4.999999999999935163, 3.750000000000003553 ) ) ;
#12781 = VECTOR ( 'NONE', #18252, 1000.000000000000000 ) ;
#12782 = CARTESIAN_POINT ( 'NONE',  ( 7.884991313526920287, -12.31730826388680633, 7.773664271103689849 ) ) ;
#12783 = LINE ( 'NONE', #324, #593 ) ;
#12784 = AXIS2_PLACEMENT_3D ( 'NONE', #8081, #22786, #6560 ) ;
#12785 = CARTESIAN_POINT ( 'NONE',  ( -6.999999995230847816, -13.21736471697163395, 9.233045673661568031 ) ) ;
#12786 = CARTESIAN_POINT ( 'NONE',  ( 37.29045043747289156, 10.91119608832001830, -10.57823792062838386 ) ) ;
#12787 = DIRECTION ( 'NONE',  ( -2.168404344971017743E-16, -1.000000000000000000, 6.982962677686261977E-15 ) ) ;
#12788 = CARTESIAN_POINT ( 'NONE',  ( 4.071447262713884463, 2.020725942163681399, 3.499999999999996003 ) ) ;
#12789 = CARTESIAN_POINT ( 'NONE',  ( -7.499999999999992895, -8.000000000000044409, 6.250000000000005329 ) ) ;
#12790 = PRODUCT_RELATED_PRODUCT_CATEGORY ( 'part', '', ( #17360 ) ) ;
#12791 = PLANE ( 'NONE',  #2580 ) ;
#12792 = FACE_OUTER_BOUND ( 'NONE', #15475, .T. ) ;
#12793 = EDGE_LOOP ( 'NONE', ( #18409, #19601, #7971, #660 ) ) ;
#12794 = EDGE_CURVE ( 'NONE', #3149, #11755, #13311, .T. ) ;
#12795 = CIRCLE ( 'NONE', #2656, 0.5000000000000022204 ) ;
#12796 = EDGE_LOOP ( 'NONE', ( #9599, #15575, #13502 ) ) ;
#12797 = CARTESIAN_POINT ( 'NONE',  ( -55.05572809000118184, -2.700000000000125855, -8.000000000000062172 ) ) ;
#12798 = CARTESIAN_POINT ( 'NONE',  ( 0.000000000000000000, 0.000000000000000000, -4.000000000000000000 ) ) ;
#12800 = ADVANCED_FACE ( 'NONE', ( #13099 ), #17936, .T. ) ;
#12799 = EDGE_LOOP ( 'NONE', ( #3603, #12270, #21388, #1573 ) ) ;
#12801 = B_SPLINE_CURVE_WITH_KNOTS ( 'NONE', 3,
 ( #7893, #15054, #494, #7439, #14947, #6020, #13191, #14607, #12960, #9432 ),
 .UNSPECIFIED., .F., .F.,
 ( 4, 2, 2, 2, 4 ),
 ( 0.001941010781631091840, 0.002456031491763887437, 0.002971052201896682600, 0.003486072912029479064, 0.004001093622162275529 ),
 .UNSPECIFIED. ) ;
#12802 = DIRECTION ( 'NONE',  ( 3.885780586188016830E-16, 4.437342591868156373E-31, -1.000000000000000000 ) ) ;
#12803 = EDGE_CURVE ( 'NONE', #7321, #5263, #21594, .T. ) ;
#12804 = CARTESIAN_POINT ( 'NONE',  ( -3.092373168850688607E-14, 59.74999999999991473, 4.500000000000008882 ) ) ;
#12805 = CARTESIAN_POINT ( 'NONE',  ( 3.972709601346602337, 2.746729940827207894, -2.374099244652752461 ) ) ;
#12806 = CARTESIAN_POINT ( 'NONE',  ( -2.500000000000002220, 3.061616997868386099E-16, -25.03750572909317285 ) ) ;
#12807 = ORIENTED_EDGE ( 'NONE', *, *, #15099, .F. ) ;
#12808 = DIRECTION ( 'NONE',  ( -1.000000000000000000, 0.000000000000000000, 0.000000000000000000 ) ) ;
#12809 = CARTESIAN_POINT ( 'NONE',  ( 73.50000000000112266, -3.999999999999809042, 1.179611963664228824E-13 ) ) ;
#12810 = DIRECTION ( 'NONE',  ( 0.000000000000000000, 0.000000000000000000, 1.000000000000000000 ) ) ;
#12811 = CARTESIAN_POINT ( 'NONE',  ( 108.2426266706970637, -13.02760560296348302, 6.500000000000019540 ) ) ;
#12812 = CARTESIAN_POINT ( 'NONE',  ( -4.000000000000045297, 1.387778780781445676E-14, 0.000000000000000000 ) ) ;
#12813 = VECTOR ( 'NONE', #18232, 1000.000000000000000 ) ;
#12814 = AXIS2_PLACEMENT_3D ( 'NONE', #21489, #23257, #7020 ) ;
#12815 = CARTESIAN_POINT ( 'NONE',  ( 4.030867648405429549, 2.329326259789358922, -2.965488570641425792 ) ) ;
#12816 = CARTESIAN_POINT ( 'NONE',  ( 77.42435809754145737, -3.999999999999809042, -6.499999999999984901 ) ) ;
#12817 =( NAMED_UNIT ( * ) SI_UNIT ( $, .STERADIAN. ) SOLID_ANGLE_UNIT ( ) );
#12818 = EDGE_CURVE ( 'NONE', #7794, #9067, #18176, .T. ) ;
#12819 = CARTESIAN_POINT ( 'NONE',  ( 3.999999999999940048, 1.941961291383530019, -0.3515519931179958424 ) ) ;
#12820 = B_SPLINE_CURVE_WITH_KNOTS ( 'NONE', 3,
 ( #21164, #15384, #3045, #22460 ),
 .UNSPECIFIED., .F., .F.,
 ( 4, 4 ),
 ( 2.380739282164649823E-07, 0.002044882221487533212 ),
 .UNSPECIFIED. ) ;
#12821 = EDGE_CURVE ( 'NONE', #23201, #11583, #17449, .T. ) ;
#12822 = APPLICATION_PROTOCOL_DEFINITION ( 'draft international standard', 'automotive_design', 1998, #3962 ) ;
#12823 = ORIENTED_EDGE ( 'NONE', *, *, #18533, .T. ) ;
#12824 = ORIENTED_EDGE ( 'NONE', *, *, #22576, .T. ) ;
#12827 = ORIENTED_EDGE ( 'NONE', *, *, #924, .F. ) ;
#12826 = ADVANCED_FACE ( 'NONE', ( #12866 ), #20052, .T. ) ;
#12825 = ORIENTED_EDGE ( 'NONE', *, *, #643, .T. ) ;
#12828 = VECTOR ( 'NONE', #11936, 1000.000000000000000 ) ;
#12829 = VECTOR ( 'NONE', #1676, 1000.000000000000000 ) ;
#12830 = ADVANCED_FACE ( 'NONE', ( #18504 ), #14973, .T. ) ;
#12831 = DIRECTION ( 'NONE',  ( -3.330669073875432643E-16, -4.437342591868153746E-31, 1.000000000000000000 ) ) ;
#12832 = LINE ( 'NONE', #2120, #3947 ) ;
#12833 = CARTESIAN_POINT ( 'NONE',  ( 118.0000000000017479, -4.000000000000058620, -5.999999999999908518 ) ) ;
#12834 = DIRECTION ( 'NONE',  ( 0.000000000000000000, 0.000000000000000000, 1.000000000000000000 ) ) ;
#12835 = FACE_BOUND ( 'NONE', #18385, .T. ) ;
#12836 = CARTESIAN_POINT ( 'NONE',  ( -12.84999999999999964, -0.5000000000000004441, 0.000000000000000000 ) ) ;
#12837 = MANIFOLD_SOLID_BREP ( 'Fillet12', #4289 ) ;
#12838 = CARTESIAN_POINT ( 'NONE',  ( -6.846097631013046581, 36.00232955766364285, -18.02039154777020613 ) ) ;
#12839 = FACE_OUTER_BOUND ( 'NONE', #771, .T. ) ;
#12840 = CARTESIAN_POINT ( 'NONE',  ( -50.65685424949267457, -7.200000000000049916, 8.000000000000035527 ) ) ;
#12841 = DIRECTION ( 'NONE',  ( 1.000000000000000000, 3.254448077276381206E-32, 1.066788928082016908E-26 ) ) ;
#12842 = CARTESIAN_POINT ( 'NONE',  ( -2.886699270652946403, 4.864326267994410813, 7.500000000000007105 ) ) ;
#12843 = DIRECTION ( 'NONE',  ( 0.000000000000000000, 0.000000000000000000, -1.000000000000000000 ) ) ;
#12844 = EDGE_CURVE ( 'NONE', #14050, #16775, #11791, .T. ) ;
#12846 = ADVANCED_FACE ( 'NONE', ( #16952 ), #16730, .F. ) ;
#12845 = PLANE ( 'NONE',  #21304 ) ;
#12847 = ADVANCED_FACE ( 'NONE', ( #7918 ), #13564, .T. ) ;
#12848 = LINE ( 'NONE', #7218, #4404 ) ;
#12849 = CIRCLE ( 'NONE', #7596, 2.099999999999999645 ) ;
#12850 = CIRCLE ( 'NONE', #2332, 6.500000000000052403 ) ;
#12851 = CARTESIAN_POINT ( 'NONE',  ( 3.999999999999936939, -0.7890432684751291781, -0.04868663549878041868 ) ) ;
#12852 = DIRECTION ( 'NONE',  ( -1.000000000000000000, 5.551115122690158919E-17, -1.001543064812511222E-16 ) ) ;
#12853 = EDGE_LOOP ( 'NONE', ( #13763, #3178, #14432 ) ) ;
#12855 = ORIENTED_EDGE ( 'NONE', *, *, #10018, .F. ) ;
#12854 = ORIENTED_EDGE ( 'NONE', *, *, #18762, .F. ) ;
#12856 = EDGE_CURVE ( 'NONE', #6445, #14430, #296, .T. ) ;
#12857 = ORIENTED_EDGE ( 'NONE', *, *, #16843, .F. ) ;
#12860 = VERTEX_POINT ( 'NONE', #4373 ) ;
#12859 = ADVANCED_FACE ( 'NONE', ( #987 ), #13337, .F. ) ;
#12858 = EDGE_LOOP ( 'NONE', ( #6439, #14885, #10338, #3760 ) ) ;
#12861 = AXIS2_PLACEMENT_3D ( 'NONE', #535, #16740, #18752 ) ;
#12862 = VERTEX_POINT ( 'NONE', #11558 ) ;
#12863 = FACE_OUTER_BOUND ( 'NONE', #4142, .T. ) ;
#12864 = ORIENTED_EDGE ( 'NONE', *, *, #15747, .F. ) ;
#12865 = ORIENTED_EDGE ( 'NONE', *, *, #13179, .F. ) ;
#12866 = FACE_OUTER_BOUND ( 'NONE', #13211, .T. ) ;
#12867 = EDGE_CURVE ( 'NONE', #20043, #14311, #13452, .T. ) ;
#12868 = AXIS2_PLACEMENT_3D ( 'NONE', #22892, #6545, #17105 ) ;
#12869 = CARTESIAN_POINT ( 'NONE',  ( 24.74999999999996447, 1.500000000000098588, -17.00000000000001066 ) ) ;
#12870 = TOROIDAL_SURFACE ( 'NONE', #17754, 7.208584908080424292, 5.000000000000000000 ) ;
#12871 = DIRECTION ( 'NONE',  ( 1.550910762415566494E-16, 1.000000000000000000, -8.135128085091684243E-31 ) ) ;
#12872 = VECTOR ( 'NONE', #17726, 1000.000000000000000 ) ;
#12873 = LINE ( 'NONE', #18746, #12486 ) ;
#12874 = CARTESIAN_POINT ( 'NONE',  ( 59.19834661797869302, 1.119475911334100182, 6.000000000000165201 ) ) ;
#12875 = CARTESIAN_POINT ( 'NONE',  ( -3.999999999708153453, 35.99999999900384751, -29.50000000000000000 ) ) ;
#12876 = CARTESIAN_POINT ( 'NONE',  ( 0.2500000000000036637, 2.000000000000001776, -17.75000000000000711 ) ) ;
#12877 = CARTESIAN_POINT ( 'NONE',  ( -3.499999999708153453, 13.99999999900385106, -25.50000000000000000 ) ) ;
#12878 = AXIS2_PLACEMENT_3D ( 'NONE', #11531, #15643, #20611 ) ;
#12879 = CARTESIAN_POINT ( 'NONE',  ( 37.51717533640845659, 10.97664592903653791, -2.308399629903466366 ) ) ;
#12880 = ORIENTED_EDGE ( 'NONE', *, *, #21677, .T. ) ;
#12881 = MANIFOLD_SOLID_BREP ( 'FlangeHexFillet', #3556 ) ;
#12882 = SURFACE_STYLE_USAGE ( .BOTH. , #16626 ) ;
#12883 = DIRECTION ( 'NONE',  ( 3.032184104443272185E-30, 1.000000000000000000, -7.395570986447005381E-32 ) ) ;
#12884 = TOROIDAL_SURFACE ( 'NONE', #3500, 6.500000000000005329, 0.5000000000000000000 ) ;
#12886 = ORIENTED_EDGE ( 'NONE', *, *, #12888, .T. ) ;
#12885 = EDGE_LOOP ( 'NONE', ( #5721, #8997, #19923, #9244 ) ) ;
#12887 = AXIS2_PLACEMENT_3D ( 'NONE', #18397, #19939, #1816 ) ;
#12888 = EDGE_CURVE ( 'NONE', #522, #7130, #20747, .T. ) ;
#12889 = VECTOR ( 'NONE', #12044, 1000.000000000000114 ) ;
#12890 = ORIENTED_EDGE ( 'NONE', *, *, #913, .T. ) ;
#12891 = ORIENTED_EDGE ( 'NONE', *, *, #21749, .F. ) ;
#12892 = VERTEX_POINT ( 'NONE', #17308 ) ;
#12893 = ORIENTED_EDGE ( 'NONE', *, *, #20481, .F. ) ;
#12894 = EDGE_CURVE ( 'NONE', #5703, #3643, #4846, .T. ) ;
#12895 = ORIENTED_EDGE ( 'NONE', *, *, #4175, .T. ) ;
#12896 = DIRECTION ( 'NONE',  ( -2.013525853228507892E-32, -6.902532920683810383E-31, 1.000000000000000000 ) ) ;
#12897 = B_SPLINE_CURVE_WITH_KNOTS ( 'NONE', 3,
 ( #7184, #7409, #5423, #12581, #19766, #14578 ),
 .UNSPECIFIED., .F., .F.,
 ( 4, 2, 4 ),
 ( 0.004904497004059944938, 0.006291728891672870860, 0.007678960779285795915 ),
 .UNSPECIFIED. ) ;
#12898 = DIRECTION ( 'NONE',  ( 4.190823558986625216E-31, -1.000000000000000000, 4.190823558986625216E-31 ) ) ;
#12899 = DIRECTION ( 'NONE',  ( -4.190823558986625216E-31, 1.000000000000000000, -4.190823558986625216E-31 ) ) ;
#12900 = VECTOR ( 'NONE', #5155, 1000.000000000000000 ) ;
#12901 = CARTESIAN_POINT ( 'NONE',  ( -1.654252653722019684, -3.663718938583052420, -0.01223254789879538000 ) ) ;
#12902 = VECTOR ( 'NONE', #10985, 999.9999999999998863 ) ;
#12903 = CARTESIAN_POINT ( 'NONE',  ( -43.46238456605041023, -4.919238815542515297, -7.500000000000007105 ) ) ;
#12904 = CYLINDRICAL_SURFACE ( 'NONE', #7930, 6.249999999999992006 ) ;
#12905 = TOROIDAL_SURFACE ( 'NONE', #19675, 5.500000000000003553, 0.5000000000000000000 ) ;
#12906 = CIRCLE ( 'NONE', #11772, 1.750000000000001554 ) ;
#12907 = CARTESIAN_POINT ( 'NONE',  ( -3.499999999708153453, 42.99999999900385461, -26.50000000000000000 ) ) ;
#12908 = CIRCLE ( 'NONE', #18172, 5.749999999999992006 ) ;
#12909 = VECTOR ( 'NONE', #15886, 1000.000000000000000 ) ;
#12910 = CARTESIAN_POINT ( 'NONE',  ( -8.079084010241013303, -2.020344040167372679, 6.665520415301724455 ) ) ;
#12911 = PLANE ( 'NONE',  #12299 ) ;
#12912 = FACE_OUTER_BOUND ( 'NONE', #6387, .T. ) ;
#12913 = CARTESIAN_POINT ( 'NONE',  ( 29.00000000029184832, 16.99999999900385461, -15.99999999999999289 ) ) ;
#12914 = DIRECTION ( 'NONE',  ( 2.013525853228507892E-32, 6.902532920683810383E-31, -1.000000000000000000 ) ) ;
#12915 = DIRECTION ( 'NONE',  ( 0.000000000000000000, 0.000000000000000000, 1.000000000000000000 ) ) ;
#12916 = AXIS2_PLACEMENT_3D ( 'NONE', #22667, #17350, #11477 ) ;
#12917 = CIRCLE ( 'NONE', #18203, 0.4999999999999999445 ) ;
#12918 = ORIENTED_EDGE ( 'NONE', *, *, #5486, .T. ) ;
#12919 = VECTOR ( 'NONE', #19373, 1000.000000000000000 ) ;
#12920 = CARTESIAN_POINT ( 'NONE',  ( -5.784122180648308742, 36.25568647312941550, -28.41463637942309362 ) ) ;
#12921 = CARTESIAN_POINT ( 'NONE',  ( -45.01801948466074776, -6.474873734152911453, -7.500000000000034639 ) ) ;
#12922 = ORIENTED_EDGE ( 'NONE', *, *, #6624, .T. ) ;
#12923 = CARTESIAN_POINT ( 'NONE',  ( 37.50000000000014921, 11.00000000000000355, -10.68301270189227559 ) ) ;
#12924 = FACE_OUTER_BOUND ( 'NONE', #10362, .T. ) ;
#12925 = CARTESIAN_POINT ( 'NONE',  ( 4.086262629614044073, -1.979770830881117494, -3.570936333571148591 ) ) ;
#12926 = DIRECTION ( 'NONE',  ( 0.7071067811865490160, 0.7071067811865460184, 1.565905175853766674E-16 ) ) ;
#12927 = CARTESIAN_POINT ( 'NONE',  ( -2.869520281200714380E-14, 4.647089433458816643, -3.572167766733388206 ) ) ;
#12928 = DIRECTION ( 'NONE',  ( 1.000000000000000000, 1.910522504832140594E-31, -5.551115123125818447E-17 ) ) ;
#12929 = DIRECTION ( 'NONE',  ( 0.000000000000000000, 0.000000000000000000, 1.000000000000000000 ) ) ;
#12930 = LINE ( 'NONE', #7185, #429 ) ;
#12931 = CARTESIAN_POINT ( 'NONE',  ( 30.00000000029184832, 2.999999999003851503, -39.00000000000000000 ) ) ;
#12932 = EDGE_CURVE ( 'NONE', #12208, #3270, #8396, .T. ) ;
#12933 = CARTESIAN_POINT ( 'NONE',  ( 6.999999999999982236, -13.02884243125068942, 9.522727272727369296 ) ) ;
#12934 = CIRCLE ( 'NONE', #17442, 5.384454397937147974 ) ;
#12935 = DIRECTION ( 'NONE',  ( 1.066786462891689527E-26, 6.656013887802287108E-31, 1.000000000000000000 ) ) ;
#12936 = CLOSED_SHELL ( 'NONE', ( #7923, #2723, #4086, #2072, #2637, #6047, #3904, #20783, #10117, #17106, #6216, #5418, #10106, #18042, #13405, #10514, #2339, #18279, #8715, #13722, #17552, #20401, #4547, #16605, #13281, #10385, #5505, #1488 ) ) ;
#12937 = AXIS2_PLACEMENT_3D ( 'NONE', #4716, #8595, #11769 ) ;
#12938 = DIRECTION ( 'NONE',  ( 0.7071067811865485719, -0.7071067811865464625, -1.010793663541191485E-16 ) ) ;
#12939 = DIRECTION ( 'NONE',  ( -2.013525853228507892E-32, -6.902532920683810383E-31, 1.000000000000000000 ) ) ;
#12940 = AXIS2_PLACEMENT_3D ( 'NONE', #17575, #21119, #1359 ) ;
#12941 = LINE ( 'NONE', #11170, #2472 ) ;
#12942 = CARTESIAN_POINT ( 'NONE',  ( 4.175326769692856210, 2.060699556488931883, -3.569236330973464266 ) ) ;
#12943 = B_SPLINE_CURVE_WITH_KNOTS ( 'NONE', 3,
 ( #4001, #20012, #12952, #21895, #5893, #5446, #7658, #19905, #149, #21561, #20252, #11182, #7325, #12720 ),
 .UNSPECIFIED., .F., .F.,
 ( 4, 2, 2, 2, 2, 2, 4 ),
 ( 0.000000000000000000, 0.001000930383652479062, 0.001501395575478720653, 0.002001860767304962461, 0.002502325959131204269, 0.003002791150957445643, 0.004003721534609925789 ),
 .UNSPECIFIED. ) ;
#12944 = PRODUCT_CONTEXT ( 'NONE', #15945, 'mechanical' ) ;
#12945 = B_SPLINE_CURVE_WITH_KNOTS ( 'NONE', 3,
 ( #1197, #20612, #3073, #6484, #6377, #22490, #1317, #6604, #10235, #17290 ),
 .UNSPECIFIED., .F., .F.,
 ( 4, 2, 2, 2, 4 ),
 ( 0.005744585894170328028, 0.006138284319911526017, 0.006531982745652724007, 0.006925681171393922864, 0.007319379597135120853 ),
 .UNSPECIFIED. ) ;
#12946 = ORIENTED_EDGE ( 'NONE', *, *, #2017, .T. ) ;
#12947 = CIRCLE ( 'NONE', #22727, 2.000000000000015543 ) ;
#12949 = ORIENTED_EDGE ( 'NONE', *, *, #19168, .T. ) ;
#12948 = ORIENTED_EDGE ( 'NONE', *, *, #9248, .T. ) ;
#12950 = TOROIDAL_SURFACE ( 'NONE', #2816, 4.500000000000000888, 0.5000000000000000000 ) ;
#12951 = DIRECTION ( 'NONE',  ( -5.551115123125782702E-16, -1.201780285297635172E-31, 1.000000000000000000 ) ) ;
#12952 = CARTESIAN_POINT ( 'NONE',  ( 7.028413389564965641, -0.6300521812368736763, 8.946655872546013910 ) ) ;
#12953 = EDGE_CURVE ( 'NONE', #12086, #3004, #21179, .T. ) ;
#12954 = CARTESIAN_POINT ( 'NONE',  ( 7.602880770961806256, -11.99349919129478614, 8.461619612152116332 ) ) ;
#12955 = EDGE_LOOP ( 'NONE', ( #20888, #10485, #22885, #2945 ) ) ;
#12956 = DIRECTION ( 'NONE',  ( -3.254448077146059901E-32, -1.000000000000000000, -6.409494854920712161E-31 ) ) ;
#12957 = DIRECTION ( 'NONE',  ( 1.454462294001240516E-30, 1.000000000000000000, 0.000000000000000000 ) ) ;
#12958 = DIRECTION ( 'NONE',  ( 5.551115123125790098E-17, 6.982962677686276177E-15, 1.000000000000000000 ) ) ;
#12959 = EDGE_CURVE ( 'NONE', #1546, #20509, #19680, .T. ) ;
#12960 = CARTESIAN_POINT ( 'NONE',  ( 1.031246673762468813, -0.5999999999999888756, 4.508537709115514325 ) ) ;
#12961 = CYLINDRICAL_SURFACE ( 'NONE', #9581, 0.4999999999999978351 ) ;
#12962 = DIRECTION ( 'NONE',  ( -1.000000000000000000, -1.776356839400250465E-15, 0.000000000000000000 ) ) ;
#12963 = CYLINDRICAL_SURFACE ( 'NONE', #10206, 0.2500000000000000000 ) ;
#12964 = CARTESIAN_POINT ( 'NONE',  ( -3.610629513653814016, 4.785505255291060855, 7.500000000000006217 ) ) ;
#12965 = CARTESIAN_POINT ( 'NONE',  ( 2.499999999999998668, 4.500000000000031974, -17.50000000000001776 ) ) ;
#12966 = DIRECTION ( 'NONE',  ( 1.753951801195068057E-17, -0.7071067811865545671, -0.7071067811865404673 ) ) ;
#12967 = CARTESIAN_POINT ( 'NONE',  ( 54.42435809754108078, -4.000000000000003553, 6.500000000000081712 ) ) ;
#12968 = VECTOR ( 'NONE', #1511, 1000.000000000000114 ) ;
#12969 = EDGE_CURVE ( 'NONE', #15940, #11081, #13279, .T. ) ;
#12970 = PRESENTATION_LAYER_ASSIGNMENT (  '', '', ( #23127 ) ) ;
#12971 = DIRECTION ( 'NONE',  ( -0.8660254037844382635, -1.951185418111810735E-16, -0.5000000000000006661 ) ) ;
#12972 = EDGE_CURVE ( 'NONE', #17687, #12422, #14032, .T. ) ;
#12973 = DIRECTION ( 'NONE',  ( -1.000000000000000000, 9.637352644315586861E-16, 0.000000000000000000 ) ) ;
#12974 = CARTESIAN_POINT ( 'NONE',  ( 7.742458795615140055, -0.7399311281350806624, 8.061568688625849077 ) ) ;
#12975 = EDGE_CURVE ( 'NONE', #15314, #2644, #6534, .T. ) ;
#12976 = EDGE_LOOP ( 'NONE', ( #8821, #1881, #858, #19114, #21834, #21703 ) ) ;
#12977 = FILL_AREA_STYLE ('',( #14504 ) ) ;
#12979 = ORIENTED_EDGE ( 'NONE', *, *, #8521, .T. ) ;
#12978 = ORIENTED_EDGE ( 'NONE', *, *, #2102, .F. ) ;
#12980 = B_SPLINE_CURVE_WITH_KNOTS ( 'NONE', 3,
 ( #8533, #4873, #17465, #23004, #20896, #4651 ),
 .UNSPECIFIED., .F., .F.,
 ( 4, 2, 4 ),
 ( 0.002336974151641583314, 0.003500975885716454093, 0.004664977619791324873 ),
 .UNSPECIFIED. ) ;
#12981 = ORIENTED_EDGE ( 'NONE', *, *, #8805, .F. ) ;
#12983 = ORIENTED_EDGE ( 'NONE', *, *, #7095, .F. ) ;
#12982 = ORIENTED_EDGE ( 'NONE', *, *, #23086, .T. ) ;
#12984 = ORIENTED_EDGE ( 'NONE', *, *, #6807, .F. ) ;
#12985 = CARTESIAN_POINT ( 'NONE',  ( -5.484827557301438894, -1.325747111984083793, 0.000000000000000000 ) ) ;
#12986 = ORIENTED_EDGE ( 'NONE', *, *, #1467, .F. ) ;
#12987 = ORIENTED_EDGE ( 'NONE', *, *, #13101, .F. ) ;
#12988 = EDGE_CURVE ( 'NONE', #21787, #12089, #6849, .T. ) ;
#12989 = CARTESIAN_POINT ( 'NONE',  ( -42.54314575050782565, -4.000000000000034639, -8.000000000000007105 ) ) ;
#12990 = FACE_OUTER_BOUND ( 'NONE', #6977, .T. ) ;
#12991 = DIRECTION ( 'NONE',  ( -1.000000000000000000, 1.550910762415566494E-16, 1.495339968488870838E-47 ) ) ;
#12992 = FACE_OUTER_BOUND ( 'NONE', #12497, .T. ) ;
#12993 = CIRCLE ( 'NONE', #5112, 2.999999999999999112 ) ;
#12994 = CARTESIAN_POINT ( 'NONE',  ( 4.175572532730935649, -2.061029303918082256, -3.569807470274393602 ) ) ;
#12995 = CARTESIAN_POINT ( 'NONE',  ( 2.298974087852387438, 1.453757124409940760, -4.750000000000023981 ) ) ;
#12996 = DIRECTION ( 'NONE',  ( 4.190823558986625216E-31, -1.000000000000000000, 4.190823558986625216E-31 ) ) ;
#12997 = EDGE_CURVE ( 'NONE', #6421, #10139, #16650, .T. ) ;
#12998 = CARTESIAN_POINT ( 'NONE',  ( 7.596194078004423034, 47.59619407671642222, -19.00000000000000355 ) ) ;
#12999 = DIRECTION ( 'NONE',  ( 3.330669073875454830E-16, 0.000000000000000000, -1.000000000000000000 ) ) ;
#13000 =( BOUNDED_SURFACE ( )  B_SPLINE_SURFACE ( 3, 2, ( 
 ( #11231, #21831, #16621 ),
 ( #18408, #21950, #18191 ),
 ( #5842, #7705, #7363 ),
 ( #3937, #9238, #9588 ),
 ( #14526, #539, #16393 ),
 ( #10878, #5718, #12879 ),
 ( #18291, #14878, #18071 ),
 ( #9357, #16508, #5605 ) ),
 .UNSPECIFIED., .F., .F., .T. ) 
 B_SPLINE_SURFACE_WITH_KNOTS ( ( 4, 2, 2, 4 ),
 ( 3, 3 ),
 ( 3.665191429188094929, 3.926990816987243615, 4.188790204786392302, 4.712388980384689674 ),
 ( 0.000000000000000000, 1.000000000000000000 ),
 .UNSPECIFIED. ) 
 GEOMETRIC_REPRESENTATION_ITEM ( )  RATIONAL_B_SPLINE_SURFACE ( (
 ( 1.000000000000000000, 0.7905694150421763711, 1.000000000000000000),
 ( 1.000000000000000000, 0.8144940154005744226, 1.000000000000000000),
 ( 1.000000000000000000, 0.8408337562111710684, 1.000000000000000000),
 ( 1.000000000000000000, 0.8912170513578273612, 1.000000000000000000),
 ( 1.000000000000000000, 0.9152160911082826145, 1.000000000000000000),
 ( 1.000000000000000000, 0.9758108578640108943, 1.000000000000000000),
 ( 1.000000000000000000, 1.000509427570078991, 1.000000000000000000),
 ( 1.000000000000000000, 1.000000000000000000, 1.000000000000000000) ) ) 
 REPRESENTATION_ITEM ( '' )  SURFACE ( )  );
#13001 = ADVANCED_FACE ( 'NONE', ( #23100 ), #10372, .T. ) ;
#13002 = CIRCLE ( 'NONE', #10723, 0.5000000000000004441 ) ;
#13003 = DIRECTION ( 'NONE',  ( 2.797982890317280824E-17, 0.6666666666666667407, -0.7453559924999300090 ) ) ;
#13004 = EDGE_CURVE ( 'NONE', #7574, #22801, #5728, .T. ) ;
#13005 = ORIENTED_EDGE ( 'NONE', *, *, #16204, .T. ) ;
#13006 = CARTESIAN_POINT ( 'NONE',  ( 63.19496167919712093, -3.291091657286249195, 6.500000000000054179 ) ) ;
#13008 = EDGE_LOOP ( 'NONE', ( #175, #5376, #10970, #17298 ) ) ;
#13007 = ORIENTED_EDGE ( 'NONE', *, *, #5862, .F. ) ;
#13009 =( REPRESENTATION_RELATIONSHIP ('NONE','NONE', #19450, #981 ) REPRESENTATION_RELATIONSHIP_WITH_TRANSFORMATION ( #16687 )SHAPE_REPRESENTATION_RELATIONSHIP( ) );
#13010 = VERTEX_POINT ( 'NONE', #22857 ) ;
#13011 = ORIENTED_EDGE ( 'NONE', *, *, #5782, .T. ) ;
#13012 = ORIENTED_EDGE ( 'NONE', *, *, #12101, .F. ) ;
#13013 = VECTOR ( 'NONE', #21167, 1000.000000000000000 ) ;
#13014 = ORIENTED_EDGE ( 'NONE', *, *, #1771, .F. ) ;
#13015 = LINE ( 'NONE', #11243, #17834 ) ;
#13016 = B_SPLINE_CURVE_WITH_KNOTS ( 'NONE', 3,
 ( #19877, #10914, #9173, #13995 ),
 .UNSPECIFIED., .F., .F.,
 ( 4, 4 ),
 ( 0.002080789711329261542, 0.004173039763574516031 ),
 .UNSPECIFIED. ) ;
#13017 = CARTESIAN_POINT ( 'NONE',  ( 42.50000000000020606, 11.00000000000000000, -12.50000000000001066 ) ) ;
#13018 = LINE ( 'NONE', #6311, #17356 ) ;
#13019 = CYLINDRICAL_SURFACE ( 'NONE', #16590, 0.8000000000000090372 ) ;
#13020 = CARTESIAN_POINT ( 'NONE',  ( 4.175813232069142344, 2.061359961916371830, 3.570380186727395433 ) ) ;
#13021 = CARTESIAN_POINT ( 'NONE',  ( -6.958039891257955745, 36.00029345514013102, -18.49999999999999645 ) ) ;
#13022 = ADVANCED_FACE ( 'NONE', ( #14142 ), #6734, .F. ) ;
#13023 = DIRECTION ( 'NONE',  ( -3.885780586188016830E-16, -4.437342591868156373E-31, 1.000000000000000000 ) ) ;
#13024 = FACE_OUTER_BOUND ( 'NONE', #10660, .T. ) ;
#13025 = CARTESIAN_POINT ( 'NONE',  ( -6.000000000000143885, -2.000000000000043521, -8.000000000000035527 ) ) ;
#13026 = CONICAL_SURFACE ( 'NONE', #5522, 4.487534009422209813, 0.08726646259971666819 ) ;
#13027 = CARTESIAN_POINT ( 'NONE',  ( -56.54644007500113645, 2.700000000000056577, -8.666666666666710483 ) ) ;
#13028 = DIRECTION ( 'NONE',  ( -3.885780586188016830E-16, -4.437342591868156373E-31, 1.000000000000000000 ) ) ;
#13029 = EDGE_CURVE ( 'NONE', #1520, #19813, #21220, .T. ) ;
#13030 = TOROIDAL_SURFACE ( 'NONE', #3630, 3.299999999999999822, 0.5000000000000000000 ) ;
#13031 = FACE_OUTER_BOUND ( 'NONE', #9909, .T. ) ;
#13032 = CARTESIAN_POINT ( 'NONE',  ( 4.033895293472003374, 1.419609371826466848, -3.500000000000009326 ) ) ;
#13033 = ORIENTED_EDGE ( 'NONE', *, *, #22180, .T. ) ;
#13034 = MANIFOLD_SOLID_BREP ( 'Slot', #19334 ) ;
#13035 = CARTESIAN_POINT ( 'NONE',  ( -6.917363703046245149, 36.00086243655339757, -26.74064357473281817 ) ) ;
#13036 = DIRECTION ( 'NONE',  ( -1.000000000000000000, 0.000000000000000000, 0.000000000000000000 ) ) ;
#13037 = ORIENTED_EDGE ( 'NONE', *, *, #18243, .F. ) ;
#13038 = CIRCLE ( 'NONE', #5902, 2.999999999999995559 ) ;
#13039 = DIRECTION ( 'NONE',  ( 8.438582421954110511E-32, 0.000000000000000000, 1.000000000000000000 ) ) ;
#13040 = DIRECTION ( 'NONE',  ( 1.000000000000000000, 2.365532012695626003E-16, 8.673617379883962502E-16 ) ) ;
#13041 = AXIS2_PLACEMENT_3D ( 'NONE', #17180, #622, #4484 ) ;
#13042 = DIRECTION ( 'NONE',  ( 1.000000000000000000, -4.440892098500650814E-16, -7.860214984771113767E-18 ) ) ;
#13043 = DIRECTION ( 'NONE',  ( 1.000000000000000000, -1.374679200952743288E-16, -2.095476499216376664E-33 ) ) ;
#13044 = AXIS2_PLACEMENT_3D ( 'NONE', #12465, #14477, #18117 ) ;
#13045 = DIRECTION ( 'NONE',  ( -0.9878135252003128475, -2.193386639427060968E-16, 0.1556420233463030045 ) ) ;
#13046 = CARTESIAN_POINT ( 'NONE',  ( 1.199999999999992628, 0.6000000000000103029, 4.543283425070376857 ) ) ;
#13047 = CARTESIAN_POINT ( 'NONE',  ( -65.00000000000046896, -6.938893903907228378E-14, 3.000000000000030198 ) ) ;
#13048 = ADVANCED_FACE ( 'NONE', ( #5319 ), #12531, .T. ) ;
#13049 = CARTESIAN_POINT ( 'NONE',  ( 8.697224362267983011, 0.000000000000000000, 6.249999999999977796 ) ) ;
#13050 = CARTESIAN_POINT ( 'NONE',  ( 7.345446946324464044, -13.78184793132693819, 7.860330092054047313 ) ) ;
#13051 = CIRCLE ( 'NONE', #17537, 2.000000000000015543 ) ;
#13052 = CYLINDRICAL_SURFACE ( 'NONE', #5164, 0.5000000000000000000 ) ;
#13053 = CARTESIAN_POINT ( 'NONE',  ( 3.974175853610000253, 3.450041667725515460, -1.156004144284047630 ) ) ;
#13054 = CARTESIAN_POINT ( 'NONE',  ( -4.000000000000003553, 0.000000000000000000, -5.600000000000000533 ) ) ;
#13055 = DIRECTION ( 'NONE',  ( -6.656013887802287108E-31, -1.000000000000000000, 3.469446951953609061E-15 ) ) ;
#13056 = EDGE_CURVE ( 'NONE', #12086, #22937, #2393, .T. ) ;
#13057 = CARTESIAN_POINT ( 'NONE',  ( 4.114405500665259119, 2.025575754679715512, -3.508400121684937201 ) ) ;
#13058 = VECTOR ( 'NONE', #5768, 1000.000000000000000 ) ;
#13059 = TOROIDAL_SURFACE ( 'NONE', #19071, 5.500000000000003553, 0.5000000000000000000 ) ;
#13060 = APPLICATION_PROTOCOL_DEFINITION ( 'draft international standard', 'automotive_design', 1998, #16293 ) ;
#13061 = EDGE_LOOP ( 'NONE', ( #3175, #15215 ) ) ;
#13062 = AXIS2_PLACEMENT_3D ( 'NONE', #1079, #19176, #17165 ) ;
#13063 = EDGE_CURVE ( 'NONE', #8988, #4164, #18134, .T. ) ;
#13064 = VECTOR ( 'NONE', #1451, 1000.000000000000000 ) ;
#13066 = ORIENTED_EDGE ( 'NONE', *, *, #184, .T. ) ;
#13065 = ORIENTED_EDGE ( 'NONE', *, *, #9354, .T. ) ;
#13067 = DIRECTION ( 'NONE',  ( -1.734723475976796642E-15, 0.000000000000000000, -1.000000000000000000 ) ) ;
#13068 = AXIS2_PLACEMENT_3D ( 'NONE', #17207, #4744, #18866 ) ;
#13069 = DIRECTION ( 'NONE',  ( 0.000000000000000000, -1.000000000000000000, 0.000000000000000000 ) ) ;
#13070 = DIRECTION ( 'NONE',  ( -1.000000000000000000, -1.144237745222090235E-17, -2.013525853228508713E-32 ) ) ;
#13071 = VECTOR ( 'NONE', #18549, 1000.000000000000000 ) ;
#13072 = DIRECTION ( 'NONE',  ( 1.000000000000000000, 0.000000000000000000, 0.000000000000000000 ) ) ;
#13073 = DIRECTION ( 'NONE',  ( 0.9706398123736300620, -2.860973184834435137E-14, 0.2405376366294562085 ) ) ;
#13074 = CIRCLE ( 'NONE', #1066, 2.550000000000003819 ) ;
#13075 = DIRECTION ( 'NONE',  ( 0.000000000000000000, -1.000000000000000000, 0.000000000000000000 ) ) ;
#13076 = CARTESIAN_POINT ( 'NONE',  ( 79.34099918003242635, -6.634323149190213265, -6.000000000000012434 ) ) ;
#13077 = CARTESIAN_POINT ( 'NONE',  ( -6.000000000000088818, 7.999999999999958256, 8.000000000000035527 ) ) ;
#13078 = DIRECTION ( 'NONE',  ( 5.551115123125818447E-17, 6.982962677686276177E-15, 1.000000000000000000 ) ) ;
#13079 = FILL_AREA_STYLE ('',( #14951 ) ) ;
#13080 = DIRECTION ( 'NONE',  ( 1.070367811204237268E-16, 0.8660254037844387076, 0.4999999999999999445 ) ) ;
#13081 = CARTESIAN_POINT ( 'NONE',  ( 3.973514160553466290, -3.435084588004190476, 1.181876024140317227 ) ) ;
#13082 = CIRCLE ( 'NONE', #17979, 6.500000000000000888 ) ;
#13083 = FACE_OUTER_BOUND ( 'NONE', #4635, .T. ) ;
#13084 = CARTESIAN_POINT ( 'NONE',  ( -66.55000000000046612, 6.188383139260622304E-14, -1.999999999999974021 ) ) ;
#13085 = CARTESIAN_POINT ( 'NONE',  ( 8.178874953434444706, -0.007851515978188753839, 6.644730819939002053 ) ) ;
#13086 = ORIENTED_EDGE ( 'NONE', *, *, #18406, .F. ) ;
#13087 = FILL_AREA_STYLE ('',( #14729 ) ) ;
#13089 = ORIENTED_EDGE ( 'NONE', *, *, #12972, .F. ) ;
#13088 = VERTEX_POINT ( 'NONE', #7544 ) ;
#13090 = ADVANCED_FACE ( 'NONE', ( #5673 ), #5020, .T. ) ;
#13091 = ORIENTED_EDGE ( 'NONE', *, *, #14411, .F. ) ;
#13092 = ORIENTED_EDGE ( 'NONE', *, *, #7052, .T. ) ;
#13094 = ORIENTED_EDGE ( 'NONE', *, *, #10356, .F. ) ;
#13093 = EDGE_LOOP ( 'NONE', ( #8900, #11316, #11056, #17508 ) ) ;
#13095 = ORIENTED_EDGE ( 'NONE', *, *, #10928, .F. ) ;
#13096 = CARTESIAN_POINT ( 'NONE',  ( 24.74999999999997158, 1.999999999999988010, -18.99999999999998224 ) ) ;
#13097 = VERTEX_POINT ( 'NONE', #11408 ) ;
#13098 = ORIENTED_EDGE ( 'NONE', *, *, #11871, .F. ) ;
#13099 = FACE_OUTER_BOUND ( 'NONE', #18219, .T. ) ;
#13100 = TOROIDAL_SURFACE ( 'NONE', #12727, 5.384454397937119552, 0.5155456020628805813 ) ;
#13101 = EDGE_CURVE ( 'NONE', #7097, #14161, #604, .T. ) ;
#13102 = AXIS2_PLACEMENT_3D ( 'NONE', #5599, #9462, #412 ) ;
#13103 = DIRECTION ( 'NONE',  ( 0.6819983600624989206, -0.7313537016191700157, 0.000000000000000000 ) ) ;
#13104 = PLANE ( 'NONE',  #14026 ) ;
#13105 = CARTESIAN_POINT ( 'NONE',  ( -65.00000000000052580, 5.551115123125782702E-14, 3.000000000000002665 ) ) ;
#13106 = EDGE_CURVE ( 'NONE', #3579, #9134, #17390, .T. ) ;
#13107 = DIRECTION ( 'NONE',  ( 2.586960666708586846E-16, -0.5000000000000013323, -0.8660254037844379305 ) ) ;
#13108 = B_SPLINE_CURVE_WITH_KNOTS ( 'NONE', 3,
 ( #4483, #9783, #8138, #737, #4356 ),
 .UNSPECIFIED., .F., .F.,
 ( 4, 1, 4 ),
 ( 0.000000000000000000, 0.002309401076758508826, 0.004618802153517017652 ),
 .UNSPECIFIED. ) ;
#13109 = CARTESIAN_POINT ( 'NONE',  ( -91.14322581977734217, 2.700000000000014833, 6.823838874241886288 ) ) ;
#13110 = CARTESIAN_POINT ( 'NONE',  ( 0.000000000000000000, -11.33467790002633180, -1.387778780781445676E-14 ) ) ;
#13111 = CARTESIAN_POINT ( 'NONE',  ( 3.961557105775345367, -1.423285172353660144, 3.499999999999970246 ) ) ;
#13112 = B_SPLINE_CURVE_WITH_KNOTS ( 'NONE', 3,
 ( #965, #15408, #8481, #11884, #2954, #8251 ),
 .UNSPECIFIED., .F., .F.,
 ( 4, 2, 4 ),
 ( 0.002365888236228051462, 0.003551327329835092354, 0.004736766423442132813 ),
 .UNSPECIFIED. ) ;
#13113 = CARTESIAN_POINT ( 'NONE',  ( 30.60000000000000142, 2.775557561562891351E-14, -2.081668171172168513E-14 ) ) ;
#13114 = CARTESIAN_POINT ( 'NONE',  ( -10.00000000000000888, -24.99999999999994671, 0.000000000000000000 ) ) ;
#13115 = DIRECTION ( 'NONE',  ( -1.000000000000000000, -3.254448077276381206E-32, -1.066788928082016908E-26 ) ) ;
#13116 = ORIENTED_EDGE ( 'NONE', *, *, #14411, .T. ) ;
#13117 = UNCERTAINTY_MEASURE_WITH_UNIT (LENGTH_MEASURE( 1.000000000000000082E-05 ), #12030, 'distance_accuracy_value', 'NONE');
#13118 = MANIFOLD_SOLID_BREP ( 'Cut-Extrude2', #15564 ) ;
#13119 = ADVANCED_FACE ( 'NONE', ( #22009 ), #6247, .T. ) ;
#13120 = AXIS2_PLACEMENT_3D ( 'NONE', #21609, #14427, #86 ) ;
#13121 = ADVANCED_FACE ( 'NONE', ( #18947 ), #13417, .T. ) ;
#13122 = AXIS2_PLACEMENT_3D ( 'NONE', #10645, #18068, #192 ) ;
#13123 = DIRECTION ( 'NONE',  ( -1.000000000000000000, 7.477632011778292156E-48, -3.885780586188017323E-16 ) ) ;
#13124 = AXIS2_PLACEMENT_3D ( 'NONE', #16411, #5856, #15006 ) ;
#13126 = ORIENTED_EDGE ( 'NONE', *, *, #14163, .F. ) ;
#13125 = ORIENTED_EDGE ( 'NONE', *, *, #1659, .T. ) ;
#13127 = ADVANCED_FACE ( 'NONE', ( #4467 ), #4116, .T. ) ;
#13128 = ORIENTED_EDGE ( 'NONE', *, *, #15004, .F. ) ;
#13129 = ORIENTED_EDGE ( 'NONE', *, *, #943, .T. ) ;
#13130 = ORIENTED_EDGE ( 'NONE', *, *, #7676, .F. ) ;
#13131 = PRESENTATION_LAYER_ASSIGNMENT (  '', '', ( #7136 ) ) ;
#13132 = EDGE_LOOP ( 'NONE', ( #21446, #13266, #11439, #13727 ) ) ;
#13133 = DIRECTION ( 'NONE',  ( 0.000000000000000000, 0.000000000000000000, -1.000000000000000000 ) ) ;
#13134 = ADVANCED_FACE ( 'NONE', ( #4341 ), #2763, .T. ) ;
#13135 = CARTESIAN_POINT ( 'NONE',  ( 73.50000000000116529, -3.999999999999809042, 2.550000000000110401 ) ) ;
#13136 = ORIENTED_EDGE ( 'NONE', *, *, #21971, .T. ) ;
#13137 = ADVANCED_FACE ( 'NONE', ( #2588 ), #487, .T. ) ;
#13138 = CARTESIAN_POINT ( 'NONE',  ( 2.775557561562891351E-14, 0.000000000000000000, -2.133974596215532316 ) ) ;
#13139 = DIRECTION ( 'NONE',  ( 7.860214984770699307E-18, -1.409037165336591006E-16, -1.000000000000000000 ) ) ;
#13140 = DIRECTION ( 'NONE',  ( -3.885780586188016830E-16, -4.437342591868156373E-31, 1.000000000000000000 ) ) ;
#13141 = DIRECTION ( 'NONE',  ( 1.000000000000000000, 1.910522504832140594E-31, -5.551115123125818447E-17 ) ) ;
#13142 = DIRECTION ( 'NONE',  ( 0.8571428571428567622, 8.935192059122191449E-16, -0.5150787536377136044 ) ) ;
#13143 = CARTESIAN_POINT ( 'NONE',  ( -6.999999999999992006, -13.02884243125068409, 9.522727272727356862 ) ) ;
#13144 = DIRECTION ( 'NONE',  ( 1.331202777560457422E-30, 1.000000000000000000, -7.395570986446985676E-31 ) ) ;
#13145 = VECTOR ( 'NONE', #22657, 1000.000000000000000 ) ;
#13146 = CARTESIAN_POINT ( 'NONE',  ( 4.330127018922110160, -5.551115123125782702E-14, -7.499999999999996447 ) ) ;
#13147 = EDGE_CURVE ( 'NONE', #6184, #13207, #13535, .T. ) ;
#13148 = AXIS2_PLACEMENT_3D ( 'NONE', #15307, #11779, #18967 ) ;
#13149 = EDGE_CURVE ( 'NONE', #7942, #690, #4578, .T. ) ;
#13150 = FILL_AREA_STYLE_COLOUR ( '', #4433 ) ;
#13151 = FACE_OUTER_BOUND ( 'NONE', #4436, .T. ) ;
#13152 = DIRECTION ( 'NONE',  ( -3.070652698126929572E-17, -1.000000000000000000, 2.869019762633796499E-16 ) ) ;
#13153 = ORIENTED_EDGE ( 'NONE', *, *, #8818, .T. ) ;
#13154 = ORIENTED_EDGE ( 'NONE', *, *, #1182, .F. ) ;
#13155 = ORIENTED_EDGE ( 'NONE', *, *, #15118, .T. ) ;
#13156 = EDGE_CURVE ( 'NONE', #8964, #3689, #14831, .T. ) ;
#13157 = CARTESIAN_POINT ( 'NONE',  ( -6.846097631013046581, 36.00232955766364285, -26.97960845222978676 ) ) ;
#13158 = CARTESIAN_POINT ( 'NONE',  ( 22.49999999999994671, 4.500000000000059508, -18.99999999999998224 ) ) ;
#13159 = ORIENTED_EDGE ( 'NONE', *, *, #14695, .T. ) ;
#13160 = VECTOR ( 'NONE', #989, 1000.000000000000000 ) ;
#13161 = LINE ( 'NONE', #12689, #11774 ) ;
#13162 = CARTESIAN_POINT ( 'NONE',  ( -56.87767137932630845, -4.163336342344337027E-14, 8.833333333333401427 ) ) ;
#13163 = CARTESIAN_POINT ( 'NONE',  ( -51.07487373415331433, 0.4180194846605325698, 7.500000000000062172 ) ) ;
#13164 = CARTESIAN_POINT ( 'NONE',  ( 77.42435809754141474, -3.999999999999809042, 6.000000000000095923 ) ) ;
#13165 = DIRECTION ( 'NONE',  ( -1.000000000000000000, 0.000000000000000000, -4.336808689941968432E-16 ) ) ;
#13166 = ADVANCED_FACE ( 'NONE', ( #20253 ), #18474, .T. ) ;
#13167 = CYLINDRICAL_SURFACE ( 'NONE', #8178, 4.750000000000000888 ) ;
#13168 = ORIENTED_EDGE ( 'NONE', *, *, #12997, .T. ) ;
#13169 = LINE ( 'NONE', #15032, #7946 ) ;
#13170 = CARTESIAN_POINT ( 'NONE',  ( 119.5756419024616690, -7.000000000000062172, -6.500000000000033751 ) ) ;
#13171 = LINE ( 'NONE', #2105, #21232 ) ;
#13172 = DIRECTION ( 'NONE',  ( 2.013525853228507892E-32, 6.902532920683810383E-31, -1.000000000000000000 ) ) ;
#13173 = CARTESIAN_POINT ( 'NONE',  ( 0.000000000000000000, 0.000000000000000000, -0.3080913168122673129 ) ) ;
#13174 = CARTESIAN_POINT ( 'NONE',  ( 2.775557561562891351E-14, 0.000000000000000000, -2.133974596215532316 ) ) ;
#13175 = CARTESIAN_POINT ( 'NONE',  ( 1.828356344711600467, 3.563200125723214651, -8.699875401248920360E-15 ) ) ;
#13176 = CARTESIAN_POINT ( 'NONE',  ( 4.030867648404226955, -3.732851566702299007, -0.5345114293585417897 ) ) ;
#13177 = AXIS2_PLACEMENT_3D ( 'NONE', #7549, #2123, #14605 ) ;
#13178 =( BOUNDED_SURFACE ( )  B_SPLINE_SURFACE ( 3, 2, ( 
 ( #5226, #8514, #10389 ),
 ( #19445, #19214, #12381 ),
 ( #10272, #15567, #22870 ),
 ( #19563, #17808, #15788 ),
 ( #17923, #3348, #3452 ),
 ( #8627, #10618, #7116 ) ),
 .UNSPECIFIED., .F., .F., .T. ) 
 B_SPLINE_SURFACE_WITH_KNOTS ( ( 4, 2, 4 ),
 ( 3, 3 ),
 ( 0.02027752710269158445, 0.02273781595091097646, 0.02519810479913037193 ),
 ( 0.000000000000000000, 1.000000000000000000 ),
 .UNSPECIFIED. ) 
 GEOMETRIC_REPRESENTATION_ITEM ( )  RATIONAL_B_SPLINE_SURFACE ( (
 ( 1.000000000000000000, 0.8047781431712803801, 1.000000000000000000),
 ( 1.000000000000000000, 0.8123773247083573290, 1.000000000000000000),
 ( 1.000000000000000000, 0.8190670192155369289, 1.000000000000000000),
 ( 1.000000000000000000, 0.8192353552911690873, 1.000000000000000000),
 ( 1.000000000000000000, 0.8126132098227178968, 1.000000000000000000),
 ( 1.000000000000000000, 0.8047712465856385888, 1.000000000000000000) ) ) 
 REPRESENTATION_ITEM ( '' )  SURFACE ( )  );
#13179 = EDGE_CURVE ( 'NONE', #21802, #20271, #8702, .T. ) ;
#13180 = CONTEXT_DEPENDENT_SHAPE_REPRESENTATION ( #11794, #1417 ) ;
#13181 = ORIENTED_EDGE ( 'NONE', *, *, #14696, .T. ) ;
#13183 = ORIENTED_EDGE ( 'NONE', *, *, #4970, .F. ) ;
#13182 = ORIENTED_EDGE ( 'NONE', *, *, #6586, .T. ) ;
#13184 = CARTESIAN_POINT ( 'NONE',  ( -42.54314575050782565, -5.300000000000037126, -8.000000000000007105 ) ) ;
#13185 = ADVANCED_FACE ( 'NONE', ( #15858 ), #17162, .F. ) ;
#13186 = DIRECTION ( 'NONE',  ( -1.000000000000000000, 4.190823558986610327E-31, -1.733449886265890494E-32 ) ) ;
#13187 = ORIENTED_EDGE ( 'NONE', *, *, #22835, .F. ) ;
#13188 = CARTESIAN_POINT ( 'NONE',  ( 4.132952817037863547, 4.063368025374519910, 3.469446951953614189E-15 ) ) ;
#13189 = DIRECTION ( 'NONE',  ( 0.000000000000000000, -0.8381404052084435730, -0.5454545454545466354 ) ) ;
#13190 = PLANE ( 'NONE',  #21905 ) ;
#13191 = CARTESIAN_POINT ( 'NONE',  ( 0.5743220282100064411, -0.5999999999999890976, 4.263778219380819579 ) ) ;
#13192 = DIRECTION ( 'NONE',  ( -0.000000000000000000, 1.000000000000000000, -0.000000000000000000 ) ) ;
#13193 = DIRECTION ( 'NONE',  ( -1.000000000000000000, -4.252453317207022018E-31, 5.551115123125818447E-17 ) ) ;
#13194 = DIRECTION ( 'NONE',  ( 1.000000000000000000, 1.424116703980846297E-16, -1.095779650622964657E-32 ) ) ;
#13195 = DIRECTION ( 'NONE',  ( -3.070652698126927723E-17, -1.000000000000000000, 4.167305704548413124E-17 ) ) ;
#13196 = CARTESIAN_POINT ( 'NONE',  ( -8.697224362267997222, -1.999999999999998224, 6.249999999999977796 ) ) ;
#13197 = CARTESIAN_POINT ( 'NONE',  ( 0.000000000000000000, -3.031088913245480576, 1.749999999999994671 ) ) ;
#13198 = CARTESIAN_POINT ( 'NONE',  ( -65.55642023346354108, 6.245004513516505540E-14, -11.87813525200309783 ) ) ;
#13199 = ORIENTED_EDGE ( 'NONE', *, *, #5238, .F. ) ;
#13200 = CIRCLE ( 'NONE', #16195, 0.5000000000000029976 ) ;
#13201 = VECTOR ( 'NONE', #9381, 1000.000000000000000 ) ;
#13203 = ORIENTED_EDGE ( 'NONE', *, *, #15817, .T. ) ;
#13202 = ORIENTED_EDGE ( 'NONE', *, *, #4114, .F. ) ;
#13204 = ORIENTED_EDGE ( 'NONE', *, *, #8358, .F. ) ;
#13205 = VERTEX_POINT ( 'NONE', #23070 ) ;
#13207 = VERTEX_POINT ( 'NONE', #19173 ) ;
#13206 = VERTEX_POINT ( 'NONE', #6823 ) ;
#13208 = ORIENTED_EDGE ( 'NONE', *, *, #2593, .T. ) ;
#13209 = CARTESIAN_POINT ( 'NONE',  ( -5.261076337303407513, -1.454929939081825108, 0.3875484812921078936 ) ) ;
#13210 = ORIENTED_EDGE ( 'NONE', *, *, #7969, .T. ) ;
#13211 = EDGE_LOOP ( 'NONE', ( #1722, #2898, #3290, #5928 ) ) ;
#13212 = SURFACE_STYLE_FILL_AREA ( #18739 ) ;
#13213 = DIRECTION ( 'NONE',  ( -0.7313537016191755669, -0.6819983600624931475, 1.169467434532365146E-15 ) ) ;
#13214 = FACE_OUTER_BOUND ( 'NONE', #21719, .T. ) ;
#13215 = SPHERICAL_SURFACE ( 'NONE', #2625, 0.5000000000000000000 ) ;
#13216 = DIRECTION ( 'NONE',  ( -4.190823558986625216E-31, 1.000000000000000000, -4.190823558986625216E-31 ) ) ;
#13217 = CARTESIAN_POINT ( 'NONE',  ( 0.000000000000000000, 0.000000000000000000, -5.294516984716112873 ) ) ;
#13218 = CARTESIAN_POINT ( 'NONE',  ( -57.28378781035998912, -2.775557561562891351E-14, 8.541666666666767327 ) ) ;
#13219 = AXIS2_PLACEMENT_3D ( 'NONE', #7724, #4073, #7954 ) ;
#13220 = AXIS2_PLACEMENT_3D ( 'NONE', #4957, #23215, #7102 ) ;
#13221 = CARTESIAN_POINT ( 'NONE',  ( 3.880214671983721608, -0.7309020039786100487, 3.499999999999969802 ) ) ;
#13222 = CYLINDRICAL_SURFACE ( 'NONE', #12861, 6.000000000000047073 ) ;
#13223 = EDGE_CURVE ( 'NONE', #11457, #21236, #2244, .T. ) ;
#13224 = FACE_OUTER_BOUND ( 'NONE', #143, .T. ) ;
#13225 = DIRECTION ( 'NONE',  ( 3.885780586188016830E-16, 4.437342591868156373E-31, -1.000000000000000000 ) ) ;
#13226 = DIRECTION ( 'NONE',  ( 5.551115123125782702E-16, 1.201780285297635172E-31, -1.000000000000000000 ) ) ;
#13227 = DIRECTION ( 'NONE',  ( 2.013525853228507892E-32, 6.902532920683810383E-31, -1.000000000000000000 ) ) ;
#13228 = ORIENTED_EDGE ( 'NONE', *, *, #3301, .F. ) ;
#13229 = AXIS2_PLACEMENT_3D ( 'NONE', #22984, #15667, #2865 ) ;
#13230 = SURFACE_STYLE_FILL_AREA ( #541 ) ;
#13232 = ORIENTED_EDGE ( 'NONE', *, *, #17001, .F. ) ;
#13231 = ORIENTED_EDGE ( 'NONE', *, *, #5455, .T. ) ;
#13233 = VERTEX_POINT ( 'NONE', #1186 ) ;
#13234 = VERTEX_POINT ( 'NONE', #15402 ) ;
#13235 = VECTOR ( 'NONE', #17341, 1000.000000000000000 ) ;
#13236 = ORIENTED_EDGE ( 'NONE', *, *, #19427, .T. ) ;
#13237 = AXIS2_PLACEMENT_3D ( 'NONE', #11699, #17101, #20892 ) ;
#13238 = CIRCLE ( 'NONE', #107, 4.750000000000000888 ) ;
#13239 = ORIENTED_EDGE ( 'NONE', *, *, #4318, .F. ) ;
#13240 = CARTESIAN_POINT ( 'NONE',  ( -6.938893903907228378E-14, 4.999999999999976907, -4.163336342344337027E-14 ) ) ;
#13241 = DIRECTION ( 'NONE',  ( -1.066786462891689527E-26, -6.656013887802287108E-31, -1.000000000000000000 ) ) ;
#13242 = ORIENTED_EDGE ( 'NONE', *, *, #23047, .T. ) ;
#13243 = FACE_OUTER_BOUND ( 'NONE', #14740, .T. ) ;
#13244 = EDGE_CURVE ( 'NONE', #2907, #1495, #1303, .T. ) ;
#13245 = AXIS2_PLACEMENT_3D ( 'NONE', #19917, #10951, #20026 ) ;
#13246 = CARTESIAN_POINT ( 'NONE',  ( 4.104070371397483541, 2.023683613428320260, 3.505122836902515360 ) ) ;
#13247 = FACE_OUTER_BOUND ( 'NONE', #22072, .T. ) ;
#13248 = CYLINDRICAL_SURFACE ( 'NONE', #7583, 2.500000000000003553 ) ;
#13249 = CARTESIAN_POINT ( 'NONE',  ( -6.999999991915196951, -11.17450167042466092, 8.700799235122007147 ) ) ;
#13250 = EDGE_CURVE ( 'NONE', #16377, #3913, #7867, .T. ) ;
#13251 = CARTESIAN_POINT ( 'NONE',  ( -8.233775472210666635, -13.45629277298747262, 7.279685395985863394 ) ) ;
#13252 = DIRECTION ( 'NONE',  ( -0.7071067811865507924, -0.7071067811865441310, -2.121016688166342479E-16 ) ) ;
#13253 = AXIS2_PLACEMENT_3D ( 'NONE', #2508, #16850, #5934 ) ;
#13254 = LINE ( 'NONE', #22320, #7660 ) ;
#13255 = AXIS2_PLACEMENT_3D ( 'NONE', #1706, #8879, #10407 ) ;
#13256 = DIRECTION ( 'NONE',  ( 0.000000000000000000, 0.000000000000000000, 1.000000000000000000 ) ) ;
#13257 = AXIS2_PLACEMENT_3D ( 'NONE', #12758, #19943, #14640 ) ;
#13258 = AXIS2_PLACEMENT_3D ( 'NONE', #8558, #16264, #18057 ) ;
#13259 = ADVANCED_FACE ( 'NONE', ( #11988 ), #13654, .F. ) ;
#13260 = CARTESIAN_POINT ( 'NONE',  ( -2.339468227445725468, -3.268109542640679432, -1.836070968115783499E-14 ) ) ;
#13261 = CARTESIAN_POINT ( 'NONE',  ( 3.878104551856319748, -0.7018542299753877112, -3.500000000000009770 ) ) ;
#13262 = EDGE_CURVE ( 'NONE', #13441, #17782, #14874, .T. ) ;
#13263 = ORIENTED_EDGE ( 'NONE', *, *, #8505, .T. ) ;
#13264 = ORIENTED_EDGE ( 'NONE', *, *, #20330, .F. ) ;
#13265 = ORIENTED_EDGE ( 'NONE', *, *, #9860, .T. ) ;
#13266 = ORIENTED_EDGE ( 'NONE', *, *, #16727, .T. ) ;
#13267 = ORIENTED_EDGE ( 'NONE', *, *, #14589, .T. ) ;
#13268 = CARTESIAN_POINT ( 'NONE',  ( 79.00000000000120792, -6.999999999999811706, 6.500000000000068390 ) ) ;
#13269 = DIRECTION ( 'NONE',  ( 1.000000000000000000, -4.437342591868175641E-31, 3.330669073875457788E-16 ) ) ;
#13270 = EDGE_LOOP ( 'NONE', ( #15675, #18731, #8644, #14284 ) ) ;
#13271 = AXIS2_PLACEMENT_3D ( 'NONE', #10816, #3538, #14000 ) ;
#13272 = DIRECTION ( 'NONE',  ( -0.1556420233463035319, 1.944076074078271124E-17, -0.9878135252003127365 ) ) ;
#13273 = AXIS2_PLACEMENT_3D ( 'NONE', #1414, #15756, #2627 ) ;
#13274 = AXIS2_PLACEMENT_3D ( 'NONE', #21683, #20137, #16240 ) ;
#13275 = DIRECTION ( 'NONE',  ( 0.000000000000000000, 0.000000000000000000, -1.000000000000000000 ) ) ;
#13276 = EDGE_CURVE ( 'NONE', #6044, #2907, #11879, .T. ) ;
#13277 = DIRECTION ( 'NONE',  ( 9.121204216617949000E-31, 1.000000000000000000, -6.982962677686261977E-15 ) ) ;
#13278 = AXIS2_PLACEMENT_3D ( 'NONE', #1332, #11788, #4844 ) ;
#13279 = CIRCLE ( 'NONE', #11016, 0.5000000000000029976 ) ;
#13280 = EDGE_CURVE ( 'NONE', #22801, #2139, #6594, .T. ) ;
#13281 = ADVANCED_FACE ( 'NONE', ( #4819 ), #1491, .T. ) ;
#13282 = CARTESIAN_POINT ( 'NONE',  ( 84.32438398889952680, -11.28140466348806470, 6.500000000000137668 ) ) ;
#13283 = CARTESIAN_POINT ( 'NONE',  ( -2.000000000000119904, -3.464101615137792134, -1.040834085586084257E-14 ) ) ;
#13284 = LINE ( 'NONE', #20234, #13936 ) ;
#13285 = CARTESIAN_POINT ( 'NONE',  ( 42.50000000000014921, 2.999999999999999112, -0.4999999999999726885 ) ) ;
#13286 = CARTESIAN_POINT ( 'NONE',  ( -43.10883117545717624, 5.299999999999998934, 8.000000000000076383 ) ) ;
#13287 = DIRECTION ( 'NONE',  ( 1.000000000000000000, -2.785515554063903297E-14, -1.815210279346915817E-30 ) ) ;
#13288 = CARTESIAN_POINT ( 'NONE',  ( 4.055492966679612010, 3.795017426214636114, -0.5629142681440425511 ) ) ;
#13289 = CARTESIAN_POINT ( 'NONE',  ( 1.387778780781445676E-14, 4.618802153517020059, -5.600000000000000533 ) ) ;
#13290 = ADVANCED_FACE ( 'NONE', ( #22827 ), #11985, .T. ) ;
#13291 = CARTESIAN_POINT ( 'NONE',  ( 1.654252653721867139, 3.663718938583046647, -0.01223254789874405647 ) ) ;
#13292 = CIRCLE ( 'NONE', #3540, 2.000000000000000000 ) ;
#13293 = EDGE_CURVE ( 'NONE', #21240, #7622, #2604, .T. ) ;
#13294 = DIRECTION ( 'NONE',  ( 1.000000000000000000, 2.220446049250314067E-16, -5.825996348268307008E-33 ) ) ;
#13295 = AXIS2_PLACEMENT_3D ( 'NONE', #18233, #7411, #11276 ) ;
#13296 = CIRCLE ( 'NONE', #6919, 0.5000000000000038858 ) ;
#13297 = VECTOR ( 'NONE', #4435, 1000.000000000000000 ) ;
#13298 = ADVANCED_FACE ( 'NONE', ( #1411 ), #8621, .F. ) ;
#13299 = CIRCLE ( 'NONE', #4259, 7.000000000000000000 ) ;
#13300 = CONTEXT_DEPENDENT_SHAPE_REPRESENTATION ( #18565, #5180 ) ;
#13301 = ORIENTED_EDGE ( 'NONE', *, *, #16707, .F. ) ;
#13303 = ORIENTED_EDGE ( 'NONE', *, *, #19341, .T. ) ;
#13302 = ORIENTED_EDGE ( 'NONE', *, *, #5652, .T. ) ;
#13304 = FACE_OUTER_BOUND ( 'NONE', #11921, .T. ) ;
#13305 = DIRECTION ( 'NONE',  ( 0.000000000000000000, 0.000000000000000000, -1.000000000000000000 ) ) ;
#13306 = AXIS2_PLACEMENT_3D ( 'NONE', #2860, #14496, #16238 ) ;
#13307 = VERTEX_POINT ( 'NONE', #5058 ) ;
#13308 = AXIS2_PLACEMENT_3D ( 'NONE', #22866, #21099, #8402 ) ;
#13309 = CARTESIAN_POINT ( 'NONE',  ( 4.175572532730939201, 4.122058607836078359, -4.513569816216541579E-15 ) ) ;
#13310 = DIRECTION ( 'NONE',  ( -4.190823558986625216E-31, 1.000000000000000000, -4.190823558986625216E-31 ) ) ;
#13311 = CIRCLE ( 'NONE', #8052, 0.4999999999999995559 ) ;
#13312 = CARTESIAN_POINT ( 'NONE',  ( 4.175813232069142344, -2.061359961916364725, 3.570380186727395433 ) ) ;
#13313 = CARTESIAN_POINT ( 'NONE',  ( -4.938244945965066357, 36.80742465210828840, -16.14556293119101937 ) ) ;
#13314 = CYLINDRICAL_SURFACE ( 'NONE', #3823, 0.4999999999999978351 ) ;
#13315 = CARTESIAN_POINT ( 'NONE',  ( -1.321505333908965962, 3.855830693249139962, -0.03421028094653124491 ) ) ;
#13316 = CARTESIAN_POINT ( 'NONE',  ( 2.775557561562891351E-14, 0.5000000000000004441, -6.499999999999950262 ) ) ;
#13317 = EDGE_CURVE ( 'NONE', #2802, #4871, #10469, .T. ) ;
#13318 = CARTESIAN_POINT ( 'NONE',  ( -2.500000000000023981, 3.506612759220730751E-15, 6.830473686658677934E-15 ) ) ;
#13319 = CARTESIAN_POINT ( 'NONE',  ( 1.446367150925026657, 4.999999999999964473, 7.500000000000007105 ) ) ;
#13320 = CARTESIAN_POINT ( 'NONE',  ( 10.49999999999999467, -12.50000000000000711, 9.250000000000063949 ) ) ;
#13321 = LINE ( 'NONE', #15301, #19475 ) ;
#13322 = DIRECTION ( 'NONE',  ( 0.000000000000000000, -6.938893903907237844E-15, -1.000000000000000000 ) ) ;
#13323 = EDGE_CURVE ( 'NONE', #15653, #16591, #17759, .T. ) ;
#13324 = VERTEX_POINT ( 'NONE', #1647 ) ;
#13325 = CIRCLE ( 'NONE', #21961, 2.499999999999993783 ) ;
#13327 = ORIENTED_EDGE ( 'NONE', *, *, #15193, .F. ) ;
#13326 = ORIENTED_EDGE ( 'NONE', *, *, #3610, .T. ) ;
#13328 = UNCERTAINTY_MEASURE_WITH_UNIT (LENGTH_MEASURE( 1.000000000000000082E-05 ), #22674, 'distance_accuracy_value', 'NONE');
#13329 = AXIS2_PLACEMENT_3D ( 'NONE', #16382, #7464, #5705 ) ;
#13330 = ORIENTED_EDGE ( 'NONE', *, *, #10397, .T. ) ;
#13331 = EDGE_LOOP ( 'NONE', ( #14728, #16259, #2145, #23147 ) ) ;
#13333 = ORIENTED_EDGE ( 'NONE', *, *, #10402, .F. ) ;
#13332 = VERTEX_POINT ( 'NONE', #8940 ) ;
#13334 = FACE_OUTER_BOUND ( 'NONE', #14195, .T. ) ;
#13335 = DIRECTION ( 'NONE',  ( 6.656013887802287108E-31, 1.000000000000000000, -3.469446951953609061E-15 ) ) ;
#13336 = VERTEX_POINT ( 'NONE', #1864 ) ;
#13337 = CYLINDRICAL_SURFACE ( 'NONE', #12567, 0.5000000000000004441 ) ;
#13338 = CARTESIAN_POINT ( 'NONE',  ( -50.65685424949275983, 2.700000000000021938, 7.500000000000062172 ) ) ;
#13339 = CYLINDRICAL_SURFACE ( 'NONE', #15145, 0.5000000000000004441 ) ;
#13340 = DIRECTION ( 'NONE',  ( 0.000000000000000000, 0.000000000000000000, -1.000000000000000000 ) ) ;
#13341 = DIRECTION ( 'NONE',  ( 0.000000000000000000, 0.000000000000000000, 1.000000000000000000 ) ) ;
#13342 = CIRCLE ( 'NONE', #6207, 0.5000000000000028866 ) ;
#13343 = CARTESIAN_POINT ( 'NONE',  ( -8.697224362268023867, -12.50000000000002842, 6.250000000000088818 ) ) ;
#13344 = DIRECTION ( 'NONE',  ( -0.2405376366294420254, 0.000000000000000000, 0.9706398123736336148 ) ) ;
#13345 = DIRECTION ( 'NONE',  ( -4.440892098500626162E-15, 0.000000000000000000, 1.000000000000000000 ) ) ;
#13346 = CARTESIAN_POINT ( 'NONE',  ( 5.599999999999994316, 4.041451884327383226, 0.000000000000000000 ) ) ;
#13347 = CARTESIAN_POINT ( 'NONE',  ( -4.000000000000003553, -1.933795701539610556, -0.2488376576623001213 ) ) ;
#13348 = CARTESIAN_POINT ( 'NONE',  ( 119.5756419024615838, -11.00000000000006573, -6.500000000000075495 ) ) ;
#13349 = CARTESIAN_POINT ( 'NONE',  ( -4.733938537004359404, 13.62597557122357372, -28.91485355091821674 ) ) ;
#13350 = DIRECTION ( 'NONE',  ( 1.431475090352998897E-31, -3.469446951953609061E-15, -1.000000000000000000 ) ) ;
#13351 = ORIENTED_EDGE ( 'NONE', *, *, #12953, .T. ) ;
#13352 = MANIFOLD_SOLID_BREP ( 'FlangeHexFillet', #21214 ) ;
#13354 = B_SPLINE_CURVE_WITH_KNOTS ( 'NONE', 3,
 ( #20134, #7667, #609, #11069, #7773, #2362, #14713, #9551, #18374, #22015 ),
 .UNSPECIFIED., .F., .F.,
 ( 4, 2, 2, 2, 4 ),
 ( 0.008920163802561163410, 0.009434751658411351383, 0.009949339514261541090, 0.01046392737011172906, 0.01097851522596191877 ),
 .UNSPECIFIED. ) ;
#13353 = SHAPE_REPRESENTATION_RELATIONSHIP ( 'NONE' , 'NONE' ,  #9834, #10311 ) ;
#13356 = ORIENTED_EDGE ( 'NONE', *, *, #3938, .T. ) ;
#13355 = VERTEX_POINT ( 'NONE', #16205 ) ;
#13357 = ORIENTED_EDGE ( 'NONE', *, *, #14971, .T. ) ;
#13358 = VERTEX_POINT ( 'NONE', #13 ) ;
#13359 = VECTOR ( 'NONE', #3415, 1000.000000000000000 ) ;
#13360 = ORIENTED_EDGE ( 'NONE', *, *, #20074, .T. ) ;
#13361 = EDGE_CURVE ( 'NONE', #22096, #12509, #7500, .T. ) ;
#13362 = ORIENTED_EDGE ( 'NONE', *, *, #6959, .F. ) ;
#13363 = DIRECTION ( 'NONE',  ( 0.000000000000000000, 0.000000000000000000, -1.000000000000000000 ) ) ;
#13364 = DIRECTION ( 'NONE',  ( 2.013525853228507892E-32, 6.902532920683810383E-31, -1.000000000000000000 ) ) ;
#13365 = ORIENTED_EDGE ( 'NONE', *, *, #3996, .F. ) ;
#13366 = FACE_OUTER_BOUND ( 'NONE', #17326, .T. ) ;
#13367 = PLANE ( 'NONE',  #13991 ) ;
#13368 = DIRECTION ( 'NONE',  ( 1.000000000000000000, 0.000000000000000000, 0.000000000000000000 ) ) ;
#13369 = CARTESIAN_POINT ( 'NONE',  ( 2.499999999999992006, 2.000000000000001776, -3.469446951953614189E-14 ) ) ;
#13370 = CARTESIAN_POINT ( 'NONE',  ( -8.181569977154559581, -11.86479625201650556, 7.340676138759481439 ) ) ;
#13371 = CARTESIAN_POINT ( 'NONE',  ( -7.796097383573772355, -13.30002726899557075, 7.943830786858237403 ) ) ;
#13372 = PLANE ( 'NONE',  #4831 ) ;
#13373 = DIRECTION ( 'NONE',  ( -1.000000000000000000, -2.699383410053119644E-30, -3.330669073875432643E-16 ) ) ;
#13374 = CARTESIAN_POINT ( 'NONE',  ( 37.86602540378469683, -6.071532165918824830E-15, -10.86602540378448722 ) ) ;
#13375 = CIRCLE ( 'NONE', #2098, 0.5000000000000004441 ) ;
#13376 = CYLINDRICAL_SURFACE ( 'NONE', #1090, 2.999999999999999112 ) ;
#13377 = DIRECTION ( 'NONE',  ( 1.000000000000000000, 0.000000000000000000, 0.000000000000000000 ) ) ;
#13378 = VERTEX_POINT ( 'NONE', #122 ) ;
#13379 = VECTOR ( 'NONE', #4911, 1000.000000000000000 ) ;
#13380 = ORIENTED_EDGE ( 'NONE', *, *, #15969, .T. ) ;
#13381 = EDGE_LOOP ( 'NONE', ( #2086, #17006, #655, #5577, #8239 ) ) ;
#13382 = VERTEX_POINT ( 'NONE', #21426 ) ;
#13383 = ADVANCED_FACE ( 'NONE', ( #9283 ), #18105, .T. ) ;
#13384 = CARTESIAN_POINT ( 'NONE',  ( -4.000000000000003553, 2.309401076758532678, -5.242734410091827613 ) ) ;
#13385 = DIRECTION ( 'NONE',  ( 4.190823558986621713E-31, 1.000000000000000000, 4.190823558986611203E-31 ) ) ;
#13386 = VERTEX_POINT ( 'NONE', #5420 ) ;
#13387 = FACE_OUTER_BOUND ( 'NONE', #21702, .T. ) ;
#13388 = CARTESIAN_POINT ( 'NONE',  ( -7.500000000000020428, -1.999999999999991340, 9.250000000000008882 ) ) ;
#13389 = EDGE_CURVE ( 'NONE', #15071, #16509, #17655, .T. ) ;
#13390 = B_SPLINE_CURVE_WITH_KNOTS ( 'NONE', 3,
 ( #16762, #3959, #2200, #438, #7609, #7727 ),
 .UNSPECIFIED., .F., .F.,
 ( 4, 2, 4 ),
 ( 0.02095135962594951370, 0.02312341562515501936, 0.02529547162436052155 ),
 .UNSPECIFIED. ) ;
#13391 = CARTESIAN_POINT ( 'NONE',  ( 4.086262629614002329, 1.979770830881015575, 3.570936333571067767 ) ) ;
#13392 = ADVANCED_FACE ( 'NONE', ( #3533 ), #10695, .F. ) ;
#13393 = CARTESIAN_POINT ( 'NONE',  ( 0.000000000000000000, 0.000000000000000000, 0.000000000000000000 ) ) ;
#13394 = EDGE_CURVE ( 'NONE', #16867, #19367, #15380, .T. ) ;
#13395 = DIRECTION ( 'NONE',  ( 2.013525853228507892E-32, 6.902532920683810383E-31, -1.000000000000000000 ) ) ;
#13396 = VECTOR ( 'NONE', #6776, 1000.000000000000000 ) ;
#13397 = CARTESIAN_POINT ( 'NONE',  ( 8.954763739086850194, -14.00000000000004263, 6.678571428571495439 ) ) ;
#13398 = CARTESIAN_POINT ( 'NONE',  ( -42.54314575050793934, 3.999999999999996447, 7.500000000000062172 ) ) ;
#13399 = COLOUR_RGB ( '', 0.66274510, 0.83137255, 0.94901961) ;
#13400 = DIRECTION ( 'NONE',  ( -1.000000000000000000, -1.479114197289388027E-30, -2.013525853228507892E-32 ) ) ;
#13401 = CONICAL_SURFACE ( 'NONE', #16037, 4.000000000000000000, 1.047197551196595855 ) ;
#13402 = DIRECTION ( 'NONE',  ( -0.7313537016191733464, 0.6819983600624954789, -3.733258675956564523E-18 ) ) ;
#13403 = DIRECTION ( 'NONE',  ( -5.551115123561405253E-17, -1.000000000000000000, -2.256980353643891447E-27 ) ) ;
#13404 = CARTESIAN_POINT ( 'NONE',  ( 124.5000000000019469, -7.000000000000062172, -2.549999999999971401 ) ) ;
#13405 = ADVANCED_FACE ( 'NONE', ( #12576 ), #5260, .T. ) ;
#13406 = EDGE_CURVE ( 'NONE', #2262, #20512, #5644, .T. ) ;
#13407 = AXIS2_PLACEMENT_3D ( 'NONE', #6793, #12308, #3274 ) ;
#13408 = ORIENTED_EDGE ( 'NONE', *, *, #18595, .F. ) ;
#13409 = AXIS2_PLACEMENT_3D ( 'NONE', #8051, #4277, #18637 ) ;
#13410 = MECHANICAL_DESIGN_GEOMETRIC_PRESENTATION_REPRESENTATION (  '', ( #13799 ), #6664 ) ;
#13412 = VERTEX_POINT ( 'NONE', #2096 ) ;
#13411 = VERTEX_POINT ( 'NONE', #18228 ) ;
#13413 = EDGE_CURVE ( 'NONE', #6303, #9707, #6463, .T. ) ;
#13414 = DIRECTION ( 'NONE',  ( 0.000000000000000000, 0.000000000000000000, 1.000000000000000000 ) ) ;
#13415 = EDGE_CURVE ( 'NONE', #15826, #18197, #8256, .T. ) ;
#13416 = DIRECTION ( 'NONE',  ( 1.000000000000000000, 0.000000000000000000, 0.000000000000000000 ) ) ;
#13417 = CYLINDRICAL_SURFACE ( 'NONE', #18174, 2.500000000000002220 ) ;
#13418 = VECTOR ( 'NONE', #8572, 1000.000000000000000 ) ;
#13420 = ORIENTED_EDGE ( 'NONE', *, *, #7109, .T. ) ;
#13419 = ADVANCED_FACE ( 'NONE', ( #3008 ), #14270, .T. ) ;
#13421 = CARTESIAN_POINT ( 'NONE',  ( -4.183059378720227706, -0.7499999999999437117, -2.875963052517019225 ) ) ;
#13422 = DIRECTION ( 'NONE',  ( 1.000000000000000000, 2.699383410053119644E-30, 3.330669073875432643E-16 ) ) ;
#13423 = PRODUCT_DEFINITION_SHAPE ( 'NONE', 'NONE',  #23287 ) ;
#13424 = EDGE_CURVE ( 'NONE', #18888, #7942, #6741, .T. ) ;
#13425 = LINE ( 'NONE', #9774, #1257 ) ;
#13426 = DIRECTION ( 'NONE',  ( 0.000000000000000000, 0.000000000000000000, -1.000000000000000000 ) ) ;
#13427 = CARTESIAN_POINT ( 'NONE',  ( -6.958621627098453431E-14, -4.618802153517120423, -3.504271511726807731 ) ) ;
#13428 = CARTESIAN_POINT ( 'NONE',  ( -12.84999999999999964, -0.5000000000000038858, 6.250000000000033751 ) ) ;
#13429 = AXIS2_PLACEMENT_3D ( 'NONE', #11741, #6802, #15502 ) ;
#13430 = DIRECTION ( 'NONE',  ( -5.551115123561405253E-17, -1.000000000000000000, -2.256980353643891447E-27 ) ) ;
#13431 = PRESENTATION_STYLE_ASSIGNMENT (( #16582 ) ) ;
#13432 = DIRECTION ( 'NONE',  ( 3.032184104443272185E-30, 1.000000000000000000, -7.395570986447005381E-32 ) ) ;
#13433 = AXIS2_PLACEMENT_3D ( 'NONE', #5161, #110, #7055 ) ;
#13434 = DIRECTION ( 'NONE',  ( -1.000000000000000000, 4.615739097524200579E-16, -1.134196829589822059E-15 ) ) ;
#13435 = VECTOR ( 'NONE', #7071, 1000.000000000000000 ) ;
#13436 = DIRECTION ( 'NONE',  ( 2.081668171172155892E-14, 0.000000000000000000, 1.000000000000000000 ) ) ;
#13437 = ORIENTED_EDGE ( 'NONE', *, *, #13548, .T. ) ;
#13438 = VECTOR ( 'NONE', #21916, 1000.000000000000000 ) ;
#13439 = ADVANCED_FACE ( 'NONE', ( #9404 ), #3978, .T. ) ;
#13441 = VERTEX_POINT ( 'NONE', #22101 ) ;
#13440 = EDGE_LOOP ( 'NONE', ( #3269, #5006, #17243, #5014 ) ) ;
#13442 = AXIS2_PLACEMENT_3D ( 'NONE', #651, #7587, #9587 ) ;
#13443 = EDGE_LOOP ( 'NONE', ( #19195, #3210, #15797, #5167 ) ) ;
#13445 = ORIENTED_EDGE ( 'NONE', *, *, #19004, .F. ) ;
#13444 = ORIENTED_EDGE ( 'NONE', *, *, #2047, .T. ) ;
#13446 = AXIS2_PLACEMENT_3D ( 'NONE', #5153, #16188, #17734 ) ;
#13447 = EDGE_CURVE ( 'NONE', #7123, #17843, #22908, .T. ) ;
#13448 = CYLINDRICAL_SURFACE ( 'NONE', #9511, 2.550000000000003819 ) ;
#13449 = CIRCLE ( 'NONE', #10822, 10.00000000000006395 ) ;
#13450 = DIRECTION ( 'NONE',  ( 0.000000000000000000, 0.000000000000000000, -1.000000000000000000 ) ) ;
#13451 = VERTEX_POINT ( 'NONE', #11702 ) ;
#13452 = LINE ( 'NONE', #20633, #19716 ) ;
#13453 = CYLINDRICAL_SURFACE ( 'NONE', #3992, 0.5000000000000000000 ) ;
#13454 = FACE_OUTER_BOUND ( 'NONE', #9882, .T. ) ;
#13455 = CARTESIAN_POINT ( 'NONE',  ( -8.954763739086814667, -1.499999999999987566, 6.678571428571395074 ) ) ;
#13456 = VECTOR ( 'NONE', #18692, 1000.000000000000227 ) ;
#13457 = DIRECTION ( 'NONE',  ( 1.000000000000000000, -4.440892098500650814E-16, -7.860214984771113767E-18 ) ) ;
#13458 = CARTESIAN_POINT ( 'NONE',  ( -2.500000000000006217, 3.191891195797315193E-15, -4.974599999999995248 ) ) ;
#13459 = PLANE ( 'NONE',  #2538 ) ;
#13460 = CARTESIAN_POINT ( 'NONE',  ( 2.918498775983380256E-10, -9.961476088449217059E-10, -26.00000000000000000 ) ) ;
#13461 = CARTESIAN_POINT ( 'NONE',  ( 2.500000000000002220, 3.061616997868386099E-16, -5.574599999999999334 ) ) ;
#13462 = DIRECTION ( 'NONE',  ( 1.000000000000000000, 3.254448077276381206E-32, 1.066788928082016908E-26 ) ) ;
#13463 = DIRECTION ( 'NONE',  ( 6.656013887802287108E-31, 1.000000000000000000, -3.469446951953609061E-15 ) ) ;
#13464 = CARTESIAN_POINT ( 'NONE',  ( -55.25320565519145788, 3.200000000000098765, 10.00000000000009237 ) ) ;
#13465 = CARTESIAN_POINT ( 'NONE',  ( -7.499999999999992895, -5.999999999999987566, 6.249999999999992006 ) ) ;
#13466 = STYLED_ITEM ( 'NONE', ( #6323 ), #3571 ) ;
#13467 = VERTEX_POINT ( 'NONE', #8302 ) ;
#13468 = PRESENTATION_STYLE_ASSIGNMENT (( #11812 ) ) ;
#13470 = ORIENTED_EDGE ( 'NONE', *, *, #2235, .F. ) ;
#13469 = ORIENTED_EDGE ( 'NONE', *, *, #6354, .F. ) ;
#13471 = VECTOR ( 'NONE', #5271, 1000.000000000000000 ) ;
#13472 = EDGE_CURVE ( 'NONE', #2644, #10463, #2221, .T. ) ;
#13473 = CIRCLE ( 'NONE', #19868, 2.549999999999997158 ) ;
#13474 = EDGE_LOOP ( 'NONE', ( #11209, #978, #8177, #2491 ) ) ;
#13475 = AXIS2_PLACEMENT_3D ( 'NONE', #2231, #9414, #14815 ) ;
#13476 = CIRCLE ( 'NONE', #7846, 0.4999999999999995559 ) ;
#13477 = ORIENTED_EDGE ( 'NONE', *, *, #18050, .T. ) ;
#13478 = EDGE_CURVE ( 'NONE', #11689, #10216, #8425, .T. ) ;
#13479 = ORIENTED_EDGE ( 'NONE', *, *, #15983, .F. ) ;
#13480 = CARTESIAN_POINT ( 'NONE',  ( 5.600000000000000533, 2.359070914220255805E-30, 2.499999999999996891 ) ) ;
#13481 = DIRECTION ( 'NONE',  ( 0.000000000000000000, 6.802837160693368935E-15, 1.000000000000000000 ) ) ;
#13482 = ORIENTED_EDGE ( 'NONE', *, *, #19301, .T. ) ;
#13483 = ORIENTED_EDGE ( 'NONE', *, *, #208, .F. ) ;
#13484 = EDGE_CURVE ( 'NONE', #16351, #17191, #16130, .T. ) ;
#13485 = DIRECTION ( 'NONE',  ( -3.885780586188016830E-16, -4.437342591868156373E-31, 1.000000000000000000 ) ) ;
#13486 = DIRECTION ( 'NONE',  ( 1.000000000000000000, 1.776356839400265611E-14, 3.717264591378832268E-16 ) ) ;
#13487 = PLANE ( 'NONE',  #9698 ) ;
#13488 = DIRECTION ( 'NONE',  ( 2.168404344971008868E-16, 1.000000000000000000, -8.890457814381136359E-15 ) ) ;
#13489 = CARTESIAN_POINT ( 'NONE',  ( 4.124214193018072905, 4.056676826581892215, 5.871626145799555152E-18 ) ) ;
#13490 = DIRECTION ( 'NONE',  ( 0.000000000000000000, 0.000000000000000000, -1.000000000000000000 ) ) ;
#13491 = CIRCLE ( 'NONE', #12784, 0.4999999999999999445 ) ;
#13492 = DIRECTION ( 'NONE',  ( 0.8191520442889886899, 0.000000000000000000, 0.5735764363510506003 ) ) ;
#13493 = CIRCLE ( 'NONE', #2978, 5.384454397937147974 ) ;
#13494 = DIRECTION ( 'NONE',  ( 2.013525853228508439E-32, 6.779273404243028164E-31, -1.000000000000000000 ) ) ;
#13495 = CARTESIAN_POINT ( 'NONE',  ( 37.86602540378463999, -6.071532165918824830E-15, -10.86602540378451032 ) ) ;
#13496 = ORIENTED_EDGE ( 'NONE', *, *, #11360, .F. ) ;
#13497 = LINE ( 'NONE', #20681, #18014 ) ;
#13498 = DIRECTION ( 'NONE',  ( 1.000000000000000000, -1.389842848855773151E-62, 2.013525853228507618E-32 ) ) ;
#13499 = ORIENTED_EDGE ( 'NONE', *, *, #1458, .F. ) ;
#13500 =( GEOMETRIC_REPRESENTATION_CONTEXT ( 3 ) GLOBAL_UNCERTAINTY_ASSIGNED_CONTEXT ( ( #3940 ) ) GLOBAL_UNIT_ASSIGNED_CONTEXT ( ( #22291, #17214, #17325 ) ) REPRESENTATION_CONTEXT ( 'NONE', 'WORKASPACE' ) );
#13501 = ORIENTED_EDGE ( 'NONE', *, *, #21542, .T. ) ;
#13502 = ORIENTED_EDGE ( 'NONE', *, *, #18856, .F. ) ;
#13503 = ORIENTED_EDGE ( 'NONE', *, *, #22174, .F. ) ;
#13504 = LINE ( 'NONE', #15020, #21888 ) ;
#13505 = CIRCLE ( 'NONE', #2233, 0.5000000000000029976 ) ;
#13506 = CARTESIAN_POINT ( 'NONE',  ( -1.318516776095816523, -3.857556137907097060, -1.903157303500181160E-14 ) ) ;
#13507 = ORIENTED_EDGE ( 'NONE', *, *, #11419, .F. ) ;
#13508 = DIRECTION ( 'NONE',  ( -1.858632295689435609E-16, -1.000000000000000000, 0.000000000000000000 ) ) ;
#13509 = CARTESIAN_POINT ( 'NONE',  ( -50.65685424949280247, 0.5000000000000213163, 8.000000000000090594 ) ) ;
#13510 = DIRECTION ( 'NONE',  ( 0.7071067811865554553, -0.7071067811865398012, 0.000000000000000000 ) ) ;
#13511 = DIRECTION ( 'NONE',  ( -2.013525853228507892E-32, -6.902532920683810383E-31, 1.000000000000000000 ) ) ;
#13512 = CARTESIAN_POINT ( 'NONE',  ( -1.387778780781445676E-14, 0.2500000000000140998, -2.000000000000001776 ) ) ;
#13513 = VECTOR ( 'NONE', #21650, 1000.000000000000000 ) ;
#13514 = DIRECTION ( 'NONE',  ( 3.032184104443272185E-30, 1.000000000000000000, -7.395570986447005381E-32 ) ) ;
#13515 = CARTESIAN_POINT ( 'NONE',  ( 2.742413778650726108, 1.750000000000001554, 4.750000000000000888 ) ) ;
#13516 = AXIS2_PLACEMENT_3D ( 'NONE', #17652, #19189, #12122 ) ;
#13517 = PRODUCT_RELATED_PRODUCT_CATEGORY ( 'part', '', ( #6477 ) ) ;
#13518 = CARTESIAN_POINT ( 'NONE',  ( 8.954763739086848418, -13.50000000000004441, 6.678571428571493662 ) ) ;
#13519 = DIRECTION ( 'NONE',  ( -1.550910762415566494E-16, -1.000000000000000000, 8.135128085091684243E-31 ) ) ;
#13520 = ORIENTED_EDGE ( 'NONE', *, *, #19999, .T. ) ;
#13521 = CARTESIAN_POINT ( 'NONE',  ( 2.081668171172168513E-14, 10.00000000000000533, 0.000000000000000000 ) ) ;
#13522 = DIRECTION ( 'NONE',  ( 5.551115123561405253E-17, 1.000000000000000000, 2.256980353643891447E-27 ) ) ;
#13523 = LINE ( 'NONE', #15505, #13379 ) ;
#13524 = EDGE_CURVE ( 'NONE', #12651, #4029, #12752, .T. ) ;
#13525 = DIRECTION ( 'NONE',  ( 0.000000000000000000, 6.802837160693368935E-15, 1.000000000000000000 ) ) ;
#13526 = ADVANCED_FACE ( 'NONE', ( #16670 ), #13599, .T. ) ;
#13527 = CIRCLE ( 'NONE', #1145, 4.000000000000045297 ) ;
#13528 = ORIENTED_EDGE ( 'NONE', *, *, #20560, .F. ) ;
#13529 = CARTESIAN_POINT ( 'NONE',  ( 3.948103430090704968, 2.682758828852379818, -2.353325403973791641 ) ) ;
#13531 = ORIENTED_EDGE ( 'NONE', *, *, #14443, .T. ) ;
#13530 = VERTEX_POINT ( 'NONE', #15583 ) ;
#13532 = EDGE_CURVE ( 'NONE', #1694, #18669, #19132, .T. ) ;
#13533 = FACE_OUTER_BOUND ( 'NONE', #12955, .T. ) ;
#13534 = FACE_OUTER_BOUND ( 'NONE', #10906, .T. ) ;
#13535 = LINE ( 'NONE', #2831, #21780 ) ;
#13536 = VERTEX_POINT ( 'NONE', #6650 ) ;
#13537 = CARTESIAN_POINT ( 'NONE',  ( 29.00000000029184832, 16.99999999900385461, -19.00000000000000355 ) ) ;
#13538 = DIRECTION ( 'NONE',  ( -1.000000000000000000, -1.424116703980846297E-16, 1.095779650622964657E-32 ) ) ;
#13539 = DIRECTION ( 'NONE',  ( -1.000000000000000000, -2.699383410053119644E-30, -3.330669073875432643E-16 ) ) ;
#13541 = ADVANCED_FACE ( 'NONE', ( #9956 ), #15350, .F. ) ;
#13540 = DIRECTION ( 'NONE',  ( 1.000000000000000000, 0.000000000000000000, 0.000000000000000000 ) ) ;
#13542 = DIRECTION ( 'NONE',  ( -1.000000000000000000, 1.276756478318923119E-15, -1.333893503340766797E-15 ) ) ;
#13543 = LINE ( 'NONE', #13428, #22999 ) ;
#13544 = VECTOR ( 'NONE', #13340, 1000.000000000000000 ) ;
#13545 = LINE ( 'NONE', #10233, #14395 ) ;
#13546 = CARTESIAN_POINT ( 'NONE',  ( -44.61801948466079182, -6.874873734152946447, -7.500000000000007105 ) ) ;
#13547 = DIRECTION ( 'NONE',  ( -0.7313537016191752338, 0.6819983600624935915, -2.002134703001231171E-15 ) ) ;
#13548 = EDGE_CURVE ( 'NONE', #10391, #9067, #12322, .T. ) ;
#13549 = DIRECTION ( 'NONE',  ( -1.000000000000000000, 4.440892098500641939E-16, 0.000000000000000000 ) ) ;
#13550 = PLANE ( 'NONE',  #16831 ) ;
#13551 = CARTESIAN_POINT ( 'NONE',  ( 0.000000000000000000, 0.000000000000000000, 0.000000000000000000 ) ) ;
#13552 = VERTEX_POINT ( 'NONE', #20786 ) ;
#13553 = ADVANCED_FACE ( 'NONE', ( #455 ), #7634, .T. ) ;
#13554 = SHAPE_REPRESENTATION_RELATIONSHIP ( 'NONE' , 'NONE' ,  #16457, #15637 ) ;
#13555 = EDGE_CURVE ( 'NONE', #1275, #9105, #18035, .T. ) ;
#13557 = VERTEX_POINT ( 'NONE', #1707 ) ;
#13556 = VERTEX_POINT ( 'NONE', #579 ) ;
#13558 = ORIENTED_EDGE ( 'NONE', *, *, #1636, .T. ) ;
#13560 = ORIENTED_EDGE ( 'NONE', *, *, #5799, .F. ) ;
#13559 = ORIENTED_EDGE ( 'NONE', *, *, #1080, .T. ) ;
#13561 = AXIS2_PLACEMENT_3D ( 'NONE', #16698, #607, #9547 ) ;
#13562 = CARTESIAN_POINT ( 'NONE',  ( -4.000000000000002665, 1.935983797701051667, -0.2494693066162282091 ) ) ;
#13563 = DIRECTION ( 'NONE',  ( -1.000000000000000000, -3.254448077276381206E-32, -1.066788928082016908E-26 ) ) ;
#13564 = PLANE ( 'NONE',  #6568 ) ;
#13565 = LINE ( 'NONE', #20749, #4009 ) ;
#13566 = LINE ( 'NONE', #16849, #21799 ) ;
#13567 = EDGE_CURVE ( 'NONE', #16331, #11922, #12014, .T. ) ;
#13568 = CARTESIAN_POINT ( 'NONE',  ( 2.000000000000029310, 3.464101615137740175, 0.000000000000000000 ) ) ;
#13569 = EDGE_CURVE ( 'NONE', #18871, #2883, #21438, .T. ) ;
#13570 = EDGE_CURVE ( 'NONE', #18328, #138, #7879, .T. ) ;
#13571 = CARTESIAN_POINT ( 'NONE',  ( 36.00000000029184832, 2.999999999003851503, -45.00000000000000000 ) ) ;
#13572 = CARTESIAN_POINT ( 'NONE',  ( 3.999999999999606537, -0.8578082829538927756, -3.433262215449805144 ) ) ;
#13573 = CARTESIAN_POINT ( 'NONE',  ( 7.161440864725725497, -2.387752514309381180, 7.973376427817429501 ) ) ;
#13574 = CARTESIAN_POINT ( 'NONE',  ( 4.158921784487742634, 2.089935040870095850, 3.499999999999996003 ) ) ;
#13575 = DIRECTION ( 'NONE',  ( -1.000000000000000000, 0.000000000000000000, -2.668805347656595124E-16 ) ) ;
#13576 = DIRECTION ( 'NONE',  ( 8.438582421954109416E-32, 0.000000000000000000, 1.000000000000000000 ) ) ;
#13577 = DIRECTION ( 'NONE',  ( -3.330669073875432643E-16, -4.437342591868153746E-31, 1.000000000000000000 ) ) ;
#13578 = CIRCLE ( 'NONE', #22589, 2.550000000000003819 ) ;
#13579 = STYLED_ITEM ( 'NONE', ( #15933 ), #20673 ) ;
#13580 = CARTESIAN_POINT ( 'NONE',  ( -12.84999999999999964, -2.000000000000001776, -2.549999999999997158 ) ) ;
#13581 = EDGE_CURVE ( 'NONE', #17067, #22937, #12768, .T. ) ;
#13582 = FACE_OUTER_BOUND ( 'NONE', #16002, .T. ) ;
#13583 = ORIENTED_EDGE ( 'NONE', *, *, #6779, .T. ) ;
#13584 = PRODUCT_DEFINITION_CONTEXT ( 'detailed design', #230, 'design' ) ;
#13585 = EDGE_CURVE ( 'NONE', #13552, #3915, #12000, .T. ) ;
#13586 =( NAMED_UNIT ( * ) PLANE_ANGLE_UNIT ( ) SI_UNIT ( $, .RADIAN. ) );
#13588 = ORIENTED_EDGE ( 'NONE', *, *, #2829, .T. ) ;
#13587 = ORIENTED_EDGE ( 'NONE', *, *, #1879, .F. ) ;
#13589 = ORIENTED_EDGE ( 'NONE', *, *, #10118, .T. ) ;
#13590 = ORIENTED_EDGE ( 'NONE', *, *, #13147, .F. ) ;
#13591 = ORIENTED_EDGE ( 'NONE', *, *, #13063, .F. ) ;
#13592 = ORIENTED_EDGE ( 'NONE', *, *, #17002, .F. ) ;
#13593 = CARTESIAN_POINT ( 'NONE',  ( 4.175813232069142344, -2.061359961916364725, 3.570380186727402538 ) ) ;
#13594 = CIRCLE ( 'NONE', #17715, 0.2500000000000003331 ) ;
#13595 = AXIS2_PLACEMENT_3D ( 'NONE', #12921, #15021, #14564 ) ;
#13596 = DIRECTION ( 'NONE',  ( -1.000000000000000000, -6.224605580259554159E-31, 2.887593071917436153E-31 ) ) ;
#13597 = ORIENTED_EDGE ( 'NONE', *, *, #12988, .F. ) ;
#13598 = ORIENTED_EDGE ( 'NONE', *, *, #325, .T. ) ;
#13599 = PLANE ( 'NONE',  #19149 ) ;
#13600 = CARTESIAN_POINT ( 'NONE',  ( -1.300449337779986339E-16, -8.271819572847249447, -11.16066016895666380 ) ) ;
#13601 = PLANE ( 'NONE',  #9112 ) ;
#13602 = CARTESIAN_POINT ( 'NONE',  ( 3.999999999999948042, 2.309401076758532678, -3.433295621305378020 ) ) ;
#13603 = DIRECTION ( 'NONE',  ( 2.775557561562886113E-17, -2.775557561562883955E-16, 1.000000000000000000 ) ) ;
#13604 = DIRECTION ( 'NONE',  ( 1.000000000000000000, 0.000000000000000000, 2.668805347656595124E-16 ) ) ;
#13605 = FACE_OUTER_BOUND ( 'NONE', #18077, .T. ) ;
#13606 = DIRECTION ( 'NONE',  ( 4.313844246609350428E-33, 6.982962677686276966E-15, 1.000000000000000000 ) ) ;
#13607 = DIRECTION ( 'NONE',  ( -1.000000000000000000, 1.445602896647327823E-16, 0.000000000000000000 ) ) ;
#13608 = ADVANCED_FACE ( 'NONE', ( #21249 ), #4993, .T. ) ;
#13609 = CARTESIAN_POINT ( 'NONE',  ( 37.51717533640845659, 0.02335407096349230438, -10.69160037009651454 ) ) ;
#13610 = ORIENTED_EDGE ( 'NONE', *, *, #13424, .T. ) ;
#13611 = DIRECTION ( 'NONE',  ( 0.000000000000000000, 0.000000000000000000, -1.000000000000000000 ) ) ;
#13612 = CARTESIAN_POINT ( 'NONE',  ( -6.999999999708142795, 38.99999999900385461, -18.50000000000000355 ) ) ;
#13613 = CIRCLE ( 'NONE', #10219, 7.000000000000000000 ) ;
#13614 = ORIENTED_EDGE ( 'NONE', *, *, #11811, .T. ) ;
#13615 = AXIS2_PLACEMENT_3D ( 'NONE', #7603, #9257, #21965 ) ;
#13616 = ADVANCED_FACE ( 'NONE', ( #17826 ), #15921, .T. ) ;
#13617 = ORIENTED_EDGE ( 'NONE', *, *, #64, .F. ) ;
#13618 = ORIENTED_EDGE ( 'NONE', *, *, #21482, .T. ) ;
#13619 = PRODUCT_DEFINITION_SHAPE ( 'NONE', 'NONE',  #9348 ) ;
#13620 = ORIENTED_EDGE ( 'NONE', *, *, #10825, .T. ) ;
#13621 = DIRECTION ( 'NONE',  ( -1.000000000000000000, -3.254448077276381206E-32, -1.066788928082016908E-26 ) ) ;
#13622 = ORIENTED_EDGE ( 'NONE', *, *, #11974, .T. ) ;
#13623 = PRESENTATION_LAYER_ASSIGNMENT (  '', '', ( #19997 ) ) ;
#13624 = CYLINDRICAL_SURFACE ( 'NONE', #21201, 0.5000000000000004441 ) ;
#13625 = FACE_OUTER_BOUND ( 'NONE', #5982, .T. ) ;
#13626 = CARTESIAN_POINT ( 'NONE',  ( 80.15235153779146060, -8.074585193523137860, 6.000000000000109246 ) ) ;
#13627 = ORIENTED_EDGE ( 'NONE', *, *, #13567, .F. ) ;
#13628 = CARTESIAN_POINT ( 'NONE',  ( -5.423466998247613802, 35.99999999900384751, -19.34679001651818098 ) ) ;
#13629 = AXIS2_PLACEMENT_3D ( 'NONE', #7354, #21481, #16273 ) ;
#13630 = CARTESIAN_POINT ( 'NONE',  ( 66.26395429947838522, 0.000000000000000000, 6.500000000000144773 ) ) ;
#13631 = CARTESIAN_POINT ( 'NONE',  ( -7.479729963940282111, -0.8034648269414370603, 9.265052153041423821 ) ) ;
#13632 = CIRCLE ( 'NONE', #3487, 4.500000000000045297 ) ;
#13633 = VECTOR ( 'NONE', #532, 1000.000000000000000 ) ;
#13634 = CIRCLE ( 'NONE', #7987, 0.4999999999999995559 ) ;
#13635 = DIRECTION ( 'NONE',  ( 1.000000000000000000, 1.424116703980846297E-16, -1.095779650622964657E-32 ) ) ;
#13636 = CARTESIAN_POINT ( 'NONE',  ( 4.071447262713884463, 2.020725942163639655, -3.499999999999996003 ) ) ;
#13637 = DIRECTION ( 'NONE',  ( -1.000000000000000000, 1.734723475976796001E-16, 0.000000000000000000 ) ) ;
#13638 = DIRECTION ( 'NONE',  ( -1.000000000000000000, 0.000000000000000000, 0.000000000000000000 ) ) ;
#13639 = DIRECTION ( 'NONE',  ( -1.387778780781445676E-14, -1.000000000000000000, 0.000000000000000000 ) ) ;
#13640 = CARTESIAN_POINT ( 'NONE',  ( -3.355112389629213876, 2.681727112203128538, -0.2256878752776726449 ) ) ;
#13641 = VERTEX_POINT ( 'NONE', #12042 ) ;
#13642 = CONICAL_SURFACE ( 'NONE', #8386, 5.560781378645605066, 1.221730476396047704 ) ;
#13643 = AXIS2_PLACEMENT_3D ( 'NONE', #732, #7897, #614 ) ;
#13644 = AXIS2_PLACEMENT_3D ( 'NONE', #4583, #2704, #11763 ) ;
#13645 = EDGE_LOOP ( 'NONE', ( #4949, #10634, #19343, #20276 ) ) ;
#13646 = AXIS2_PLACEMENT_3D ( 'NONE', #6885, #23249, #5113 ) ;
#13647 = VECTOR ( 'NONE', #15629, 1000.000000000000000 ) ;
#13648 = CIRCLE ( 'NONE', #20419, 6.000000000000000000 ) ;
#13650 = EDGE_LOOP ( 'NONE', ( #1803, #5578, #18023, #21838 ) ) ;
#13649 = ORIENTED_EDGE ( 'NONE', *, *, #18423, .F. ) ;
#13651 = DIRECTION ( 'NONE',  ( -3.330669073875432643E-16, -4.437342591868153746E-31, 1.000000000000000000 ) ) ;
#13652 = LINE ( 'NONE', #11877, #10713 ) ;
#13653 = ADVANCED_FACE ( 'NONE', ( #14176, #23130 ), #17940, .T. ) ;
#13654 = CYLINDRICAL_SURFACE ( 'NONE', #7, 6.999999999999999112 ) ;
#13655 = ORIENTED_EDGE ( 'NONE', *, *, #8562, .T. ) ;
#13656 = CARTESIAN_POINT ( 'NONE',  ( 3.469446951953614189E-15, 0.2500000000000002220, -17.00000000000000711 ) ) ;
#13657 = DIRECTION ( 'NONE',  ( -1.000000000000000000, 2.168404344971005170E-16, -1.203141491611682442E-30 ) ) ;
#13658 = CARTESIAN_POINT ( 'NONE',  ( -92.25000000000066791, 3.200000000000056577, -2.000000000000001776 ) ) ;
#13659 = CARTESIAN_POINT ( 'NONE',  ( -6.938893903907228378E-14, 4.999999999999976907, -4.163336342344337027E-14 ) ) ;
#13660 = AXIS2_PLACEMENT_3D ( 'NONE', #5277, #4504, #6930 ) ;
#13661 = CARTESIAN_POINT ( 'NONE',  ( -2.339468227445725024, -3.268109542640679432, -5.599999999999982769 ) ) ;
#13662 = B_SPLINE_CURVE_WITH_KNOTS ( 'NONE', 3,
 ( #16339, #18009, #5184, #10587, #23192 ),
 .UNSPECIFIED., .F., .F.,
 ( 4, 1, 4 ),
 ( 0.000000000000000000, 0.002309401076758509259, 0.004618802153517018519 ),
 .UNSPECIFIED. ) ;
#13663 = VECTOR ( 'NONE', #14116, 1000.000000000000000 ) ;
#13664 = DIRECTION ( 'NONE',  ( -1.000000000000000000, 4.190823558986610327E-31, -1.733449886265890494E-32 ) ) ;
#13665 = VECTOR ( 'NONE', #19733, 1000.000000000000114 ) ;
#13666 = CYLINDRICAL_SURFACE ( 'NONE', #22432, 0.5000000000000022204 ) ;
#13667 = AXIS2_PLACEMENT_3D ( 'NONE', #11152, #21759, #4195 ) ;
#13668 = DIRECTION ( 'NONE',  ( 0.7313537016191731244, -0.6819983600624958120, 5.924440990721420203E-17 ) ) ;
#13669 = CARTESIAN_POINT ( 'NONE',  ( 37.43301270189239460, 0.2500000000000002220, -9.999999999999953815 ) ) ;
#13670 = EDGE_LOOP ( 'NONE', ( #22183, #22890, #18587, #20154 ) ) ;
#13671 = DIRECTION ( 'NONE',  ( 0.8142930928559054538, -0.5804539248959940112, 6.444318783988556354E-17 ) ) ;
#13673 = EDGE_LOOP ( 'NONE', ( #7318, #22706, #19271 ) ) ;
#13672 = ORIENTED_EDGE ( 'NONE', *, *, #1528, .F. ) ;
#13674 = VERTEX_POINT ( 'NONE', #12399 ) ;
#13675 = EDGE_CURVE ( 'NONE', #18441, #9593, #738, .T. ) ;
#13676 = AXIS2_PLACEMENT_3D ( 'NONE', #17837, #1483, #3139 ) ;
#13678 = ORIENTED_EDGE ( 'NONE', *, *, #19207, .T. ) ;
#13677 = ORIENTED_EDGE ( 'NONE', *, *, #18281, .T. ) ;
#13679 = CONICAL_SURFACE ( 'NONE', #928, 4.499999999999988454, 0.7853981633974396193 ) ;
#13680 = CARTESIAN_POINT ( 'NONE',  ( 7.949747468597695210, 47.94974746730969173, -18.50000000000000355 ) ) ;
#13681 = AXIS2_PLACEMENT_3D ( 'NONE', #13240, #20424, #9952 ) ;
#13682 = DIRECTION ( 'NONE',  ( 1.000000000000000000, 1.479114197289397135E-31, 5.916456789157588541E-31 ) ) ;
#13683 = EDGE_CURVE ( 'NONE', #3406, #12422, #20660, .T. ) ;
#13684 = PRESENTATION_STYLE_ASSIGNMENT (( #1675 ) ) ;
#13685 = LINE ( 'NONE', #22858, #4723 ) ;
#13686 = CARTESIAN_POINT ( 'NONE',  ( 33.94974746859769255, 21.94974746730969528, -19.49999999999998934 ) ) ;
#13687 = CARTESIAN_POINT ( 'NONE',  ( -7.263517083688543430, -2.279413854694210428, 7.724990489865457555 ) ) ;
#13688 = DIRECTION ( 'NONE',  ( -1.135604581876758782E-15, 6.128431095930851481E-14, 1.000000000000000000 ) ) ;
#13689 = ADVANCED_FACE ( 'NONE', ( #10290 ), #5356, .F. ) ;
#13690 = CARTESIAN_POINT ( 'NONE',  ( 3.999999999999978240, 0.8378280264232709218, -3.220590601395822983 ) ) ;
#13691 = CARTESIAN_POINT ( 'NONE',  ( 8.181569977154431683, -2.135203747983557498, 7.340676138759591574 ) ) ;
#13692 = EDGE_CURVE ( 'NONE', #6467, #15165, #19468, .T. ) ;
#13693 = CARTESIAN_POINT ( 'NONE',  ( 3.958491816110800254, 1.406739583088997048, 3.499999999999968470 ) ) ;
#13694 = CARTESIAN_POINT ( 'NONE',  ( 8.660254037844344666, -2.775557561562891351E-14, 2.081668171172168513E-14 ) ) ;
#13695 = EDGE_CURVE ( 'NONE', #5105, #11001, #14286, .T. ) ;
#13696 = DIRECTION ( 'NONE',  ( -1.000000000000000000, -1.910522504832140594E-31, 5.551115123125818447E-17 ) ) ;
#13697 = AXIS2_PLACEMENT_3D ( 'NONE', #13798, #15663, #22863 ) ;
#13698 = CLOSED_SHELL ( 'NONE', ( #9108, #3030, #2905, #12298, #19709, #18039, #6285, #4133, #15277, #8510, #9798, #3038 ) ) ;
#13699 = CIRCLE ( 'NONE', #4231, 0.5000000000000017764 ) ;
#13700 = DIRECTION ( 'NONE',  ( 0.000000000000000000, 0.000000000000000000, -1.000000000000000000 ) ) ;
#13701 = DIRECTION ( 'NONE',  ( -1.134196829589822059E-15, -6.741645191078037727E-32, 1.000000000000000000 ) ) ;
#13702 = CARTESIAN_POINT ( 'NONE',  ( 4.086262841041383709, 2.102637316508702447, -3.500000000000006217 ) ) ;
#13703 = VERTEX_POINT ( 'NONE', #23003 ) ;
#13705 = ORIENTED_EDGE ( 'NONE', *, *, #18000, .T. ) ;
#13704 = ORIENTED_EDGE ( 'NONE', *, *, #18595, .T. ) ;
#13706 = ORIENTED_EDGE ( 'NONE', *, *, #16417, .F. ) ;
#13707 = ADVANCED_FACE ( 'NONE', ( #11097 ), #7353, .T. ) ;
#13708 = ORIENTED_EDGE ( 'NONE', *, *, #6485, .T. ) ;
#13709 = ORIENTED_EDGE ( 'NONE', *, *, #23182, .T. ) ;
#13710 = ORIENTED_EDGE ( 'NONE', *, *, #15820, .T. ) ;
#13711 = AXIS2_PLACEMENT_3D ( 'NONE', #21544, #3196, #10476 ) ;
#13712 = CARTESIAN_POINT ( 'NONE',  ( -12.85000000000001386, -12.00000000000006928, 4.163336342344337027E-14 ) ) ;
#13713 = EDGE_CURVE ( 'NONE', #7460, #11432, #13527, .T. ) ;
#13714 = ORIENTED_EDGE ( 'NONE', *, *, #16456, .T. ) ;
#13715 = DIRECTION ( 'NONE',  ( 0.000000000000000000, 0.000000000000000000, 1.000000000000000000 ) ) ;
#13716 = LINE ( 'NONE', #8304, #13235 ) ;
#13717 = ADVANCED_FACE ( 'NONE', ( #185 ), #3016, .T. ) ;
#13718 = DIRECTION ( 'NONE',  ( -2.013525853228507892E-32, -6.902532920683810383E-31, 1.000000000000000000 ) ) ;
#13719 = FACE_OUTER_BOUND ( 'NONE', #13008, .T. ) ;
#13720 = CARTESIAN_POINT ( 'NONE',  ( -6.959810536856695151, 36.00015702695179698, -18.51059057611807646 ) ) ;
#13721 = DIRECTION ( 'NONE',  ( -3.885780586188016830E-16, -4.437342591868156373E-31, 1.000000000000000000 ) ) ;
#13722 = ADVANCED_FACE ( 'NONE', ( #18283 ), #4124, .T. ) ;
#13723 = CARTESIAN_POINT ( 'NONE',  ( -45.91923881554277642, 2.462384566050156209, 7.500000000000047962 ) ) ;
#13724 = DIRECTION ( 'NONE',  ( -1.000000000000000000, 4.615739097524200579E-16, 1.134196829589820086E-15 ) ) ;
#13725 = DIRECTION ( 'NONE',  ( 3.885780586188016830E-16, 4.437342591868156373E-31, -1.000000000000000000 ) ) ;
#13726 = DIRECTION ( 'NONE',  ( 8.438582421954109416E-32, 0.000000000000000000, 1.000000000000000000 ) ) ;
#13727 = ORIENTED_EDGE ( 'NONE', *, *, #14038, .F. ) ;
#13728 = CIRCLE ( 'NONE', #5074, 6.000000000000047073 ) ;
#13729 = CARTESIAN_POINT ( 'NONE',  ( 3.974175853609982934, 2.726149789692692504, 2.409821656223242847 ) ) ;
#13730 = AXIS2_PLACEMENT_3D ( 'NONE', #17278, #14940, #15171 ) ;
#13731 = CARTESIAN_POINT ( 'NONE',  ( 2.775557561562891351E-14, 8.000000000000003553, -15.49999999999998579 ) ) ;
#13732 = ORIENTED_EDGE ( 'NONE', *, *, #13478, .F. ) ;
#13733 = EDGE_LOOP ( 'NONE', ( #7369, #1865 ) ) ;
#13734 = ORIENTED_EDGE ( 'NONE', *, *, #22202, .F. ) ;
#13735 = VERTEX_POINT ( 'NONE', #287 ) ;
#13736 = ORIENTED_EDGE ( 'NONE', *, *, #591, .T. ) ;
#13737 = DIRECTION ( 'NONE',  ( 1.000000000000000000, 4.252453317207022894E-31, -5.551115123125818447E-17 ) ) ;
#13738 = FACE_OUTER_BOUND ( 'NONE', #18825, .T. ) ;
#13739 = VERTEX_POINT ( 'NONE', #7579 ) ;
#13740 = AXIS2_PLACEMENT_3D ( 'NONE', #5396, #19850, #16414 ) ;
#13741 = DIRECTION ( 'NONE',  ( -5.551115123125761132E-17, 1.577721810442025713E-30, -1.000000000000000000 ) ) ;
#13742 = EDGE_CURVE ( 'NONE', #19898, #11147, #3397, .T. ) ;
#13743 = CARTESIAN_POINT ( 'NONE',  ( 42.50000000000020606, 10.49999999999999822, -12.50000000000001066 ) ) ;
#13744 = DIRECTION ( 'NONE',  ( -1.000000000000000000, -1.910522504832140594E-31, 5.551115123125818447E-17 ) ) ;
#13745 = ORIENTED_EDGE ( 'NONE', *, *, #13447, .F. ) ;
#13746 = CARTESIAN_POINT ( 'NONE',  ( -5.384454397937147974, 7.534042519137932791E-15, -4.484454397937126302 ) ) ;
#13747 = CARTESIAN_POINT ( 'NONE',  ( 3.950241966887813483, 2.668221755853961596, 2.378504353000647331 ) ) ;
#13748 = EDGE_CURVE ( 'NONE', #19870, #8087, #12632, .T. ) ;
#13749 = CARTESIAN_POINT ( 'NONE',  ( -8.510464245293276164, -0.5071972189927809183, 6.988717072693961363 ) ) ;
#13750 = EDGE_CURVE ( 'NONE', #13530, #16094, #19163, .T. ) ;
#13751 = DIRECTION ( 'NONE',  ( 0.000000000000000000, 1.000000000000000000, 0.000000000000000000 ) ) ;
#13752 = LINE ( 'NONE', #1057, #671 ) ;
#13753 = CIRCLE ( 'NONE', #3606, 0.5000000000000004441 ) ;
#13754 = DIRECTION ( 'NONE',  ( -2.775557561562824791E-17, 0.000000000000000000, -1.000000000000000000 ) ) ;
#13755 = CARTESIAN_POINT ( 'NONE',  ( 61.48996577904083694, -5.119475911334187224, 6.000000000000067502 ) ) ;
#13756 = VECTOR ( 'NONE', #9384, 1000.000000000000000 ) ;
#13757 = CARTESIAN_POINT ( 'NONE',  ( -67.40537636629490237, -1.249000902703301108E-13, 12.70639812373640432 ) ) ;
#13758 = ORIENTED_EDGE ( 'NONE', *, *, #2867, .F. ) ;
#13759 = EDGE_LOOP ( 'NONE', ( #2035, #9820, #13037, #2085 ) ) ;
#13760 =( REPRESENTATION_RELATIONSHIP ('NONE','NONE', #19450, #9834 ) REPRESENTATION_RELATIONSHIP_WITH_TRANSFORMATION ( #20707 )SHAPE_REPRESENTATION_RELATIONSHIP( ) );
#13762 = VERTEX_POINT ( 'NONE', #18510 ) ;
#13761 = ORIENTED_EDGE ( 'NONE', *, *, #22202, .T. ) ;
#13763 = ORIENTED_EDGE ( 'NONE', *, *, #7586, .T. ) ;
#13764 = CARTESIAN_POINT ( 'NONE',  ( 1.387778780781445676E-14, -22.49999999999995737, -2.775557561562891351E-14 ) ) ;
#13765 = ADVANCED_FACE ( 'NONE', ( #11222 ), #19536, .T. ) ;
#13766 = DIRECTION ( 'NONE',  ( -3.070652698126927723E-17, -1.000000000000000000, 4.167305704548413124E-17 ) ) ;
#13767 = AXIS2_PLACEMENT_3D ( 'NONE', #19480, #19591, #7146 ) ;
#13768 = CARTESIAN_POINT ( 'NONE',  ( -43.06238456605038323, -5.319238815542544074, -8.000000000000007105 ) ) ;
#13769 = EDGE_LOOP ( 'NONE', ( #3716, #22037, #19777, #16662 ) ) ;
#13770 = CARTESIAN_POINT ( 'NONE',  ( -12.84999999999999964, -0.5000000000000038858, 6.250000000000033751 ) ) ;
#13771 = CARTESIAN_POINT ( 'NONE',  ( 3.880358743661374010, -1.739972214219160263, 2.779021504384370900 ) ) ;
#13772 = DIRECTION ( 'NONE',  ( -0.000000000000000000, -0.000000000000000000, 1.000000000000000000 ) ) ;
#13773 = ADVANCED_FACE ( 'NONE', ( #2397 ), #10868, .T. ) ;
#13774 = CARTESIAN_POINT ( 'NONE',  ( 2.498001805406602216E-13, 3.000000000000002665, 6.000000000000158096 ) ) ;
#13775 = DIRECTION ( 'NONE',  ( 5.551115123125782702E-16, 3.966469614587832056E-31, 1.000000000000000000 ) ) ;
#13776 = DIRECTION ( 'NONE',  ( 1.000000000000000000, 1.771896121890576795E-14, 3.717264591378832268E-16 ) ) ;
#13777 = CARTESIAN_POINT ( 'NONE',  ( -6.999999999708142795, 35.99999999900384751, -26.00000000000000000 ) ) ;
#13778 = CARTESIAN_POINT ( 'NONE',  ( 12.84999999999997300, -0.5000000000000004441, 5.750000000000018652 ) ) ;
#13779 = AXIS2_PLACEMENT_3D ( 'NONE', #21037, #2563, #11729 ) ;
#13780 = CARTESIAN_POINT ( 'NONE',  ( -42.54314575050795355, 5.299999999999991829, -7.500000000000007105 ) ) ;
#13781 = ORIENTED_EDGE ( 'NONE', *, *, #8790, .F. ) ;
#13782 = VECTOR ( 'NONE', #20532, 1000.000000000000000 ) ;
#13783 = EDGE_CURVE ( 'NONE', #13762, #16689, #21941, .T. ) ;
#13784 = DIRECTION ( 'NONE',  ( 0.5804539248959940112, 0.8142930928559052317, 1.116298917846945500E-11 ) ) ;
#13786 = ORIENTED_EDGE ( 'NONE', *, *, #13983, .F. ) ;
#13785 = ORIENTED_EDGE ( 'NONE', *, *, #19578, .F. ) ;
#13787 = UNCERTAINTY_MEASURE_WITH_UNIT (LENGTH_MEASURE( 1.000000000000000082E-05 ), #7026, 'distance_accuracy_value', 'NONE');
#13788 = ORIENTED_EDGE ( 'NONE', *, *, #2235, .T. ) ;
#13790 = ORIENTED_EDGE ( 'NONE', *, *, #926, .T. ) ;
#13789 = ORIENTED_EDGE ( 'NONE', *, *, #8005, .T. ) ;
#13791 = DIRECTION ( 'NONE',  ( 0.000000000000000000, 0.000000000000000000, -1.000000000000000000 ) ) ;
#13792 = LINE ( 'NONE', #2975, #19712 ) ;
#13793 = CARTESIAN_POINT ( 'NONE',  ( 124.5000000000018332, -6.500000000000061284, -5.999999999999943157 ) ) ;
#13794 = CYLINDRICAL_SURFACE ( 'NONE', #2846, 2.500000000000002220 ) ;
#13795 = LINE ( 'NONE', #10605, #2642 ) ;
#13796 = LINE ( 'NONE', #19326, #22666 ) ;
#13797 = CIRCLE ( 'NONE', #7802, 0.5000000000000018874 ) ;
#13798 = CARTESIAN_POINT ( 'NONE',  ( 66.26395429947838522, 0.000000000000000000, 6.500000000000144773 ) ) ;
#13799 = STYLED_ITEM ( 'NONE', ( #16102 ), #21055 ) ;
#13800 = CARTESIAN_POINT ( 'NONE',  ( 0.000000000000000000, 0.000000000000000000, -0.3080913168122673129 ) ) ;
#13801 = CARTESIAN_POINT ( 'NONE',  ( 4.086262418390197659, -2.102635014057361307, 3.499999999999995559 ) ) ;
#13802 = DIRECTION ( 'NONE',  ( 3.254448077146059901E-32, 1.000000000000000000, 6.409494854920712161E-31 ) ) ;
#13803 = CARTESIAN_POINT ( 'NONE',  ( -12.85000000000005649, -13.50000000000011191, -6.249999999999921840 ) ) ;
#13804 = TOROIDAL_SURFACE ( 'NONE', #8165, 9.499999999999998224, 0.5000000000000000000 ) ;
#13805 = DIRECTION ( 'NONE',  ( 1.000000000000000000, 2.220446049250313081E-16, -3.656342123407104498E-48 ) ) ;
#13806 = DIRECTION ( 'NONE',  ( 9.121204216617949000E-31, 1.000000000000000000, -6.982962677686261977E-15 ) ) ;
#13807 = CARTESIAN_POINT ( 'NONE',  ( 4.030867648405966008, -2.329326259789339382, 2.965488570641001687 ) ) ;
#13808 = PRODUCT ( 'Hold Down Arm', 'Hold Down Arm', '', ( #369 ) ) ;
#13809 = ORIENTED_EDGE ( 'NONE', *, *, #1471, .F. ) ;
#13810 = EDGE_CURVE ( 'NONE', #13843, #11435, #17271, .T. ) ;
#13811 = VECTOR ( 'NONE', #8226, 1000.000000000000000 ) ;
#13813 = EDGE_LOOP ( 'NONE', ( #11954, #13588, #6902, #12474 ) ) ;
#13812 = ORIENTED_EDGE ( 'NONE', *, *, #1597, .T. ) ;
#13814 = CIRCLE ( 'NONE', #15662, 4.000000000000022204 ) ;
#13815 = ORIENTED_EDGE ( 'NONE', *, *, #7092, .T. ) ;
#13816 = EDGE_CURVE ( 'NONE', #16719, #18130, #5707, .T. ) ;
#13817 = ORIENTED_EDGE ( 'NONE', *, *, #18878, .T. ) ;
#13818 = VECTOR ( 'NONE', #4933, 1000.000000000000000 ) ;
#13819 = VERTEX_POINT ( 'NONE', #642 ) ;
#13820 = EDGE_CURVE ( 'NONE', #16720, #6492, #3926, .T. ) ;
#13821 = ORIENTED_EDGE ( 'NONE', *, *, #10028, .T. ) ;
#13822 = DIRECTION ( 'NONE',  ( -9.693457064947022734E-26, 0.000000000000000000, 1.000000000000000000 ) ) ;
#13823 = CIRCLE ( 'NONE', #10809, 2.549999999999997158 ) ;
#13824 = CARTESIAN_POINT ( 'NONE',  ( -2.700000000000091216, 1.999999999999911626, 7.500000000000034639 ) ) ;
#13825 = ORIENTED_EDGE ( 'NONE', *, *, #18898, .F. ) ;
#13826 = CARTESIAN_POINT ( 'NONE',  ( 0.3126073911695753660, -2.020725942163847932, -3.499999999999975131 ) ) ;
#13827 = DIRECTION ( 'NONE',  ( 2.172745813409348851E-17, -1.000000000000000000, -3.406761633869148826E-16 ) ) ;
#13828 = PLANE ( 'NONE',  #12490 ) ;
#13829 = CARTESIAN_POINT ( 'NONE',  ( 29.00000000029184832, 16.99999999900385461, -25.50000000000000355 ) ) ;
#13830 = DIRECTION ( 'NONE',  ( -1.000000000000000000, 1.365024226554777796E-62, -2.013525853228508439E-32 ) ) ;
#13831 = CYLINDRICAL_SURFACE ( 'NONE', #1375, 2.500000000000003997 ) ;
#13832 = AXIS2_PLACEMENT_3D ( 'NONE', #21805, #5810, #12973 ) ;
#13833 = ADVANCED_FACE ( 'NONE', ( #529 ), #22549, .T. ) ;
#13834 = DIRECTION ( 'NONE',  ( 1.000000000000000000, 1.479114197289397135E-31, 5.916456789157588541E-31 ) ) ;
#13835 = CARTESIAN_POINT ( 'NONE',  ( 2.742413778650726108, 1.325747111984056037, 4.749999999999997335 ) ) ;
#13836 = CARTESIAN_POINT ( 'NONE',  ( 37.69160037009659447, 0.02335407096354361403, -10.51717533640881364 ) ) ;
#13837 = ORIENTED_EDGE ( 'NONE', *, *, #22604, .F. ) ;
#13838 = EDGE_CURVE ( 'NONE', #22909, #9299, #2044, .T. ) ;
#13839 = CARTESIAN_POINT ( 'NONE',  ( -1.734723475976807094E-14, 2.000000000000001776, -17.00000000000000711 ) ) ;
#13840 = VECTOR ( 'NONE', #9294, 1000.000000000000000 ) ;
#13841 = CARTESIAN_POINT ( 'NONE',  ( 2.775557561562891351E-14, -1.387778780781445676E-14, -12.50000000000001066 ) ) ;
#13843 = VERTEX_POINT ( 'NONE', #19818 ) ;
#13842 = EDGE_LOOP ( 'NONE', ( #18391, #22342 ) ) ;
#13844 = EDGE_CURVE ( 'NONE', #6978, #7176, #22176, .T. ) ;
#13845 = ORIENTED_EDGE ( 'NONE', *, *, #16268, .T. ) ;
#13846 = ADVANCED_FACE ( 'NONE', ( #16272 ), #14977, .T. ) ;
#13847 = ORIENTED_EDGE ( 'NONE', *, *, #17007, .T. ) ;
#13848 =( GEOMETRIC_REPRESENTATION_CONTEXT ( 3 ) GLOBAL_UNCERTAINTY_ASSIGNED_CONTEXT ( ( #19927 ) ) GLOBAL_UNIT_ASSIGNED_CONTEXT ( ( #16888, #4424, #10081 ) ) REPRESENTATION_CONTEXT ( 'NONE', 'WORKASPACE' ) );
#13849 = LINE ( 'NONE', #15721, #10981 ) ;
#13850 = CARTESIAN_POINT ( 'NONE',  ( 5.550000000291854363, 42.99999999900385461, -15.99999999999999289 ) ) ;
#13851 = ORIENTED_EDGE ( 'NONE', *, *, #16727, .F. ) ;
#13852 = LINE ( 'NONE', #12307, #10977 ) ;
#13853 = DIRECTION ( 'NONE',  ( 1.000000000000000000, 0.000000000000000000, 0.000000000000000000 ) ) ;
#13854 = LINE ( 'NONE', #19376, #19619 ) ;
#13855 = VECTOR ( 'NONE', #13611, 1000.000000000000000 ) ;
#13856 = EDGE_CURVE ( 'NONE', #8962, #8469, #20521, .T. ) ;
#13857 = CARTESIAN_POINT ( 'NONE',  ( 4.180345304246171345, 4.135116856707326427, -0.02129519942693453363 ) ) ;
#13858 = TOROIDAL_SURFACE ( 'NONE', #1447, 3.500000000000000000, 0.5000000000000000000 ) ;
#13859 = EDGE_CURVE ( 'NONE', #6130, #20921, #9690, .T. ) ;
#13860 = CARTESIAN_POINT ( 'NONE',  ( -3.999999999708153453, 42.99999999900385461, -26.50000000000000000 ) ) ;
#13861 = ADVANCED_FACE ( 'NONE', ( #15435 ), #13215, .F. ) ;
#13862 = LINE ( 'NONE', #9033, #15959 ) ;
#13863 = EDGE_CURVE ( 'NONE', #17750, #7689, #10149, .T. ) ;
#13864 = LINE ( 'NONE', #12073, #17190 ) ;
#13865 = CYLINDRICAL_SURFACE ( 'NONE', #9526, 2.500000000000006661 ) ;
#13866 = DIRECTION ( 'NONE',  ( -0.8191520442889886899, 1.003171929053520926E-16, 0.5735764363510506003 ) ) ;
#13867 = CARTESIAN_POINT ( 'NONE',  ( 2.918498775983380256E-10, 2.999999999003851503, -19.00000000000000355 ) ) ;
#13868 = DIRECTION ( 'NONE',  ( -1.331202777560457422E-30, -1.000000000000000000, 7.395570986446985676E-31 ) ) ;
#13869 = EDGE_LOOP ( 'NONE', ( #19137, #20507, #7093, #10363 ) ) ;
#13870 = EDGE_CURVE ( 'NONE', #2421, #16051, #9926, .T. ) ;
#13871 = TOROIDAL_SURFACE ( 'NONE', #5985, 2.500000000000003997, 0.5000000000000000000 ) ;
#13872 = EDGE_CURVE ( 'NONE', #7853, #7223, #15080, .T. ) ;
#13873 = EDGE_LOOP ( 'NONE', ( #22583, #9744 ) ) ;
#13874 = DIRECTION ( 'NONE',  ( -1.000000000000000000, -1.479114197289397135E-31, -5.916456789157588541E-31 ) ) ;
#13876 = VERTEX_POINT ( 'NONE', #2980 ) ;
#13875 = ORIENTED_EDGE ( 'NONE', *, *, #11242, .F. ) ;
#13877 = AXIS2_PLACEMENT_3D ( 'NONE', #1249, #4650, #8186 ) ;
#13878 = DIRECTION ( 'NONE',  ( -7.395570986446975166E-31, -3.382522293539642681E-32, -1.000000000000000000 ) ) ;
#13879 = EDGE_LOOP ( 'NONE', ( #8880, #14967, #2410, #11872, #8491 ) ) ;
#13880 = MECHANICAL_DESIGN_GEOMETRIC_PRESENTATION_REPRESENTATION (  '', ( #22518 ), #1472 ) ;
#13881 = DIRECTION ( 'NONE',  ( 1.000000000000000000, 4.252453317207022018E-31, -5.551115123125818447E-17 ) ) ;
#13882 = CARTESIAN_POINT ( 'NONE',  ( 3.191035955565536320, -1.584759246591021187, -3.972963596181403378 ) ) ;
#13883 = ORIENTED_EDGE ( 'NONE', *, *, #18439, .F. ) ;
#13884 = DIRECTION ( 'NONE',  ( 4.190823558986626092E-31, -1.000000000000000000, -4.190823558986610327E-31 ) ) ;
#13885 = DIRECTION ( 'NONE',  ( 0.000000000000000000, 1.000000000000000000, 0.000000000000000000 ) ) ;
#13886 = DIRECTION ( 'NONE',  ( -1.000000000000000000, -4.252453317207022018E-31, 5.551115123125818447E-17 ) ) ;
#13887 = CARTESIAN_POINT ( 'NONE',  ( 4.000000000000003553, 0.000000000000000000, 0.000000000000000000 ) ) ;
#13888 = LINE ( 'NONE', #19293, #10696 ) ;
#13889 = FACE_OUTER_BOUND ( 'NONE', #6495, .T. ) ;
#13890 = DIRECTION ( 'NONE',  ( -1.066786462891689527E-26, -6.656013887802287108E-31, -1.000000000000000000 ) ) ;
#13891 = CARTESIAN_POINT ( 'NONE',  ( -42.54314575050782565, -4.000000000000034639, -8.000000000000007105 ) ) ;
#13892 = EDGE_CURVE ( 'NONE', #15346, #7035, #13566, .T. ) ;
#13893 = DIRECTION ( 'NONE',  ( 3.032184104443272185E-30, 1.000000000000000000, -7.395570986447005381E-32 ) ) ;
#13894 = AXIS2_PLACEMENT_3D ( 'NONE', #3699, #21597, #14516 ) ;
#13895 = PRODUCT_DEFINITION_FORMATION_WITH_SPECIFIED_SOURCE ( 'ANY', '', #6477, .NOT_KNOWN. ) ;
#13896 = ORIENTED_EDGE ( 'NONE', *, *, #17948, .T. ) ;
#13897 = DIRECTION ( 'NONE',  ( -0.9426737730613098387, -0.3337156837524328790, -1.360023205165816762E-15 ) ) ;
#13899 = ORIENTED_EDGE ( 'NONE', *, *, #22962, .T. ) ;
#13898 = EDGE_LOOP ( 'NONE', ( #2147, #4980, #18725 ) ) ;
#13900 = EDGE_CURVE ( 'NONE', #22503, #16146, #16148, .T. ) ;
#13901 = ORIENTED_EDGE ( 'NONE', *, *, #16785, .F. ) ;
#13903 = ORIENTED_EDGE ( 'NONE', *, *, #10928, .T. ) ;
#13902 = ORIENTED_EDGE ( 'NONE', *, *, #12388, .F. ) ;
#13904 = DIRECTION ( 'NONE',  ( -2.168404344971017743E-16, 1.000000000000000000, 1.287063703585503763E-46 ) ) ;
#13905 = DIRECTION ( 'NONE',  ( -1.000000000000000000, -1.479114197289397135E-31, -5.916456789157588541E-31 ) ) ;
#13906 =( NAMED_UNIT ( * ) SI_UNIT ( $, .STERADIAN. ) SOLID_ANGLE_UNIT ( ) );
#13907 = DIRECTION ( 'NONE',  ( 0.000000000000000000, -1.000000000000000000, 0.000000000000000000 ) ) ;
#13908 = AXIS2_PLACEMENT_3D ( 'NONE', #7209, #9312, #18030 ) ;
#13909 = LINE ( 'NONE', #4848, #7040 ) ;
#13910 = LINE ( 'NONE', #4961, #1889 ) ;
#13911 = CARTESIAN_POINT ( 'NONE',  ( 2.500000000000000000, 2.570099380655439722E-14, 17.24999999999997513 ) ) ;
#13912 = CARTESIAN_POINT ( 'NONE',  ( 4.071447262713884463, 2.020725942163688504, 3.499999999999997780 ) ) ;
#13913 = DIRECTION ( 'NONE',  ( 0.5833333333333275972, 1.380506584136762077E-30, -0.8122328620674178490 ) ) ;
#13914 = CARTESIAN_POINT ( 'NONE',  ( 4.055498735588828119, -1.410041617599661290, 3.568038744583681865 ) ) ;
#13915 = CARTESIAN_POINT ( 'NONE',  ( 12.49999999999995914, 2.775557561562891351E-14, -9.500000000000003553 ) ) ;
#13916 = FACE_OUTER_BOUND ( 'NONE', #10277, .T. ) ;
#13917 = DIRECTION ( 'NONE',  ( -1.000000000000000000, 0.000000000000000000, 0.000000000000000000 ) ) ;
#13918 = CYLINDRICAL_SURFACE ( 'NONE', #8194, 4.000000000000045297 ) ;
#13919 = DIRECTION ( 'NONE',  ( 1.000000000000000000, -1.550910762415513985E-16, -3.012982189080959477E-32 ) ) ;
#13920 = ORIENTED_EDGE ( 'NONE', *, *, #19458, .T. ) ;
#13921 =( LENGTH_UNIT ( ) NAMED_UNIT ( * ) SI_UNIT ( .MILLI., .METRE. ) );
#13922 = CIRCLE ( 'NONE', #3773, 4.366025403784456138 ) ;
#13924 = ORIENTED_EDGE ( 'NONE', *, *, #1392, .T. ) ;
#13923 = EDGE_LOOP ( 'NONE', ( #11603, #11004, #14708, #21921, #5193, #1695 ) ) ;
#13925 = ORIENTED_EDGE ( 'NONE', *, *, #17478, .F. ) ;
#13926 = ORIENTED_EDGE ( 'NONE', *, *, #3761, .T. ) ;
#13927 = ORIENTED_EDGE ( 'NONE', *, *, #3116, .F. ) ;
#13928 = ORIENTED_EDGE ( 'NONE', *, *, #16709, .F. ) ;
#13929 = DIRECTION ( 'NONE',  ( 0.000000000000000000, 0.000000000000000000, 1.000000000000000000 ) ) ;
#13930 = DIRECTION ( 'NONE',  ( -9.121204216617949000E-31, -1.000000000000000000, 6.982962677686261977E-15 ) ) ;
#13931 = ORIENTED_EDGE ( 'NONE', *, *, #14425, .T. ) ;
#13932 = CARTESIAN_POINT ( 'NONE',  ( -6.999999999999992006, -5.999999999999987566, 6.250000000000005329 ) ) ;
#13933 = CARTESIAN_POINT ( 'NONE',  ( 0.3461262719735577198, -4.658553426539340236, -3.671615880910400254 ) ) ;
#13934 = ADVANCED_FACE ( 'NONE', ( #6509 ), #6279, .T. ) ;
#13935 = DIRECTION ( 'NONE',  ( -1.000000000000000000, 0.000000000000000000, -3.330669073875408978E-16 ) ) ;
#13936 = VECTOR ( 'NONE', #20463, 1000.000000000000000 ) ;
#13937 = AXIS2_PLACEMENT_3D ( 'NONE', #18211, #21848, #9610 ) ;
#13938 = LINE ( 'NONE', #7986, #21196 ) ;
#13939 = FACE_OUTER_BOUND ( 'NONE', #8636, .T. ) ;
#13940 = CARTESIAN_POINT ( 'NONE',  ( -1.839530896184778719, -1.562503694739640014, 4.749999999999998224 ) ) ;
#13941 = PLANE ( 'NONE',  #16844 ) ;
#13942 = CARTESIAN_POINT ( 'NONE',  ( -5.945013150601170970, 13.92153864138982300, -16.70732315498745635 ) ) ;
#13943 = CARTESIAN_POINT ( 'NONE',  ( -7.595478965369684587, -2.023942297479878416, 8.489833260407415594 ) ) ;
#13944 = EDGE_LOOP ( 'NONE', ( #18272, #4983, #4308, #3264 ) ) ;
#13945 = PRESENTATION_STYLE_ASSIGNMENT (( #10656 ) ) ;
#13946 = CARTESIAN_POINT ( 'NONE',  ( 4.175813232069142344, 2.061359961916364725, -3.570380186727397209 ) ) ;
#13947 = CARTESIAN_POINT ( 'NONE',  ( 6.999999999999978684, -12.60977222864647196, 9.250000000000092371 ) ) ;
#13949 = EDGE_LOOP ( 'NONE', ( #15188, #16747, #16833, #21269 ) ) ;
#13948 = VERTEX_POINT ( 'NONE', #10036 ) ;
#13950 = EDGE_LOOP ( 'NONE', ( #14340, #1431, #1357, #14507 ) ) ;
#13951 = CIRCLE ( 'NONE', #22236, 2.250000000000003109 ) ;
#13952 = VECTOR ( 'NONE', #10603, 1000.000000000000114 ) ;
#13953 = ORIENTED_EDGE ( 'NONE', *, *, #5098, .F. ) ;
#13954 = ORIENTED_EDGE ( 'NONE', *, *, #10933, .F. ) ;
#13955 = DIRECTION ( 'NONE',  ( 1.000000000000000000, 6.224605580259554159E-31, -2.887593071917436153E-31 ) ) ;
#13956 = EDGE_CURVE ( 'NONE', #7176, #6978, #9419, .T. ) ;
#13957 = CARTESIAN_POINT ( 'NONE',  ( 12.49999999999996625, 0.2500000000000002220, -9.500000000000003553 ) ) ;
#13958 = CARTESIAN_POINT ( 'NONE',  ( 7.733764002503170865, -0.7473006511613611291, 8.082002268151491364 ) ) ;
#13959 = CARTESIAN_POINT ( 'NONE',  ( 4.086262629614028086, 4.082406995609991540, 0.07093633357110795679 ) ) ;
#13960 = CARTESIAN_POINT ( 'NONE',  ( 0.02993401039715783488, -2.688325911136484336, 2.343682934607788315 ) ) ;
#13961 = EDGE_CURVE ( 'NONE', #21586, #955, #16525, .T. ) ;
#13962 = CARTESIAN_POINT ( 'NONE',  ( 6.000000000291855429, 2.999999999003851503, -5.999999999999998224 ) ) ;
#13963 = CARTESIAN_POINT ( 'NONE',  ( 0.000000000000000000, 0.000000000000000000, -5.600000000000000533 ) ) ;
#13964 = CARTESIAN_POINT ( 'NONE',  ( -9.714451465470119729E-14, 1.999999999999932498, -7.500000000000062172 ) ) ;
#13965 = CARTESIAN_POINT ( 'NONE',  ( 36.00000000029184832, 5.999999999003851059, -32.00000000000000000 ) ) ;
#13966 = CARTESIAN_POINT ( 'NONE',  ( 22.50000000000003908, 4.500000000000031974, -1.249999999999997558 ) ) ;
#13967 = DIRECTION ( 'NONE',  ( -0.000000000000000000, -0.000000000000000000, 1.000000000000000000 ) ) ;
#13968 = ADVANCED_FACE ( 'NONE', ( #8279 ), #8655, .T. ) ;
#13969 = VECTOR ( 'NONE', #7019, 1000.000000000000000 ) ;
#13970 = AXIS2_PLACEMENT_3D ( 'NONE', #6651, #1138, #19230 ) ;
#13971 = ADVANCED_FACE ( 'NONE', ( #15203 ), #15410, .T. ) ;
#13972 = CARTESIAN_POINT ( 'NONE',  ( 7.499999999999978684, -2.645898033750298417, 9.250000000000021316 ) ) ;
#13973 = DIRECTION ( 'NONE',  ( 1.066786462891689527E-26, 6.656013887802287108E-31, 1.000000000000000000 ) ) ;
#13974 = CARTESIAN_POINT ( 'NONE',  ( 30.00000000029184832, -0.5000000009961480529, -36.45000000000000284 ) ) ;
#13975 = LINE ( 'NONE', #11628, #16442 ) ;
#13976 = DIRECTION ( 'NONE',  ( -1.000000000000000000, 1.550910762415513985E-16, 3.012982189080959477E-32 ) ) ;
#13977 = ORIENTED_EDGE ( 'NONE', *, *, #16191, .F. ) ;
#13978 = AXIS2_PLACEMENT_3D ( 'NONE', #1227, #12251, #12143 ) ;
#13979 = VERTEX_POINT ( 'NONE', #22275 ) ;
#13980 = EDGE_CURVE ( 'NONE', #12125, #18888, #18744, .T. ) ;
#13981 = FACE_OUTER_BOUND ( 'NONE', #10193, .T. ) ;
#13982 = ADVANCED_FACE ( 'NONE', ( #13454 ), #5284, .T. ) ;
#13983 = EDGE_CURVE ( 'NONE', #1430, #11848, #40, .T. ) ;
#13985 = ORIENTED_EDGE ( 'NONE', *, *, #623, .F. ) ;
#13984 = VERTEX_POINT ( 'NONE', #3333 ) ;
#13986 = B_SPLINE_CURVE_WITH_KNOTS ( 'NONE', 3,
 ( #4418, #9966, #6083, #19021, #15234, #15124 ),
 .UNSPECIFIED., .F., .F.,
 ( 4, 2, 4 ),
 ( 0.002044882221487523237, 0.003063384235218489810, 0.004081886248949456383 ),
 .UNSPECIFIED. ) ;
#13987 = AXIS2_PLACEMENT_3D ( 'NONE', #1338, #12139, #22396 ) ;
#13988 = LINE ( 'NONE', #19634, #11400 ) ;
#13989 = VECTOR ( 'NONE', #11613, 999.9999999999998863 ) ;
#13990 = ORIENTED_EDGE ( 'NONE', *, *, #22199, .F. ) ;
#13991 = AXIS2_PLACEMENT_3D ( 'NONE', #22543, #10068, #15465 ) ;
#13992 = DIRECTION ( 'NONE',  ( 1.550910762415566494E-16, 1.000000000000000000, -8.135128085091684243E-31 ) ) ;
#13993 = CARTESIAN_POINT ( 'NONE',  ( 87.68350880954425008, -11.67918431276149249, 6.500000000000179412 ) ) ;
#13994 = EDGE_LOOP ( 'NONE', ( #13014, #19005, #15801, #12624 ) ) ;
#13995 = CARTESIAN_POINT ( 'NONE',  ( 4.175813232069142344, -2.061359961916364725, 3.570380186727395433 ) ) ;
#13996 = LINE ( 'NONE', #6368, #15354 ) ;
#13997 = EDGE_CURVE ( 'NONE', #5668, #9452, #13795, .T. ) ;
#13998 = CARTESIAN_POINT ( 'NONE',  ( 0.2499999999999655276, 1.500000000000056843, 0.000000000000000000 ) ) ;
#13999 = PRODUCT ( 'Nut', 'Nut', '', ( #245 ) ) ;
#14000 = DIRECTION ( 'NONE',  ( 0.000000000000000000, 0.000000000000000000, -1.000000000000000000 ) ) ;
#14001 = CARTESIAN_POINT ( 'NONE',  ( -6.591949208711866959E-14, 4.250000000000017764, -18.75000000000001066 ) ) ;
#14002 = EDGE_CURVE ( 'NONE', #14457, #17272, #12241, .T. ) ;
#14003 = CIRCLE ( 'NONE', #18499, 2.550000000000003819 ) ;
#14004 = DIRECTION ( 'NONE',  ( -1.000000000000000000, 4.190823558986610327E-31, -1.733449886265890494E-32 ) ) ;
#14005 = DIRECTION ( 'NONE',  ( 1.000000000000000000, 2.699383410053119644E-30, 3.330669073875432643E-16 ) ) ;
#14007 = ADVANCED_FACE ( 'NONE', ( #14264 ), #1519, .T. ) ;
#14006 = CARTESIAN_POINT ( 'NONE',  ( 30.60000000000000142, 2.775557561562891351E-14, -2.081668171172168513E-14 ) ) ;
#14008 =( NAMED_UNIT ( * ) SI_UNIT ( $, .STERADIAN. ) SOLID_ANGLE_UNIT ( ) );
#14009 = VECTOR ( 'NONE', #12958, 1000.000000000000000 ) ;
#14010 = CARTESIAN_POINT ( 'NONE',  ( 4.132952817037863547, -4.063368025374519910, 0.000000000000000000 ) ) ;
#14011 = AXIS2_PLACEMENT_3D ( 'NONE', #11586, #13241, #1135 ) ;
#14012 = VERTEX_POINT ( 'NONE', #3562 ) ;
#14013 = TOROIDAL_SURFACE ( 'NONE', #872, 2.500000000000000000, 0.5000000000000000000 ) ;
#14014 = DIRECTION ( 'NONE',  ( -0.9317170057714820874, -0.3631851059118813008, 1.110223024625156540E-16 ) ) ;
#14016 = ORIENTED_EDGE ( 'NONE', *, *, #2239, .F. ) ;
#14015 = EDGE_LOOP ( 'NONE', ( #13927, #21528 ) ) ;
#14017 = ORIENTED_EDGE ( 'NONE', *, *, #19319, .T. ) ;
#14019 = VERTEX_POINT ( 'NONE', #21334 ) ;
#14018 = ORIENTED_EDGE ( 'NONE', *, *, #12703, .T. ) ;
#14020 = DIRECTION ( 'NONE',  ( -4.003208021484906984E-16, 0.000000000000000000, 1.000000000000000000 ) ) ;
#14021 = DIRECTION ( 'NONE',  ( -2.887593071917436153E-31, -7.888609052210128564E-31, 1.000000000000000000 ) ) ;
#14022 = AXIS2_PLACEMENT_3D ( 'NONE', #15619, #6233, #22351 ) ;
#14023 = DIRECTION ( 'NONE',  ( -1.000000000000000000, -2.699383410053119644E-30, -3.330669073875432643E-16 ) ) ;
#14024 = CIRCLE ( 'NONE', #8413, 6.999999999999999112 ) ;
#14025 = DIRECTION ( 'NONE',  ( 1.000000000000000000, 0.000000000000000000, 0.000000000000000000 ) ) ;
#14026 = AXIS2_PLACEMENT_3D ( 'NONE', #19289, #19175, #7808 ) ;
#14027 = EDGE_CURVE ( 'NONE', #6998, #13536, #3407, .T. ) ;
#14028 = DIRECTION ( 'NONE',  ( -1.000000000000000000, 4.615739097524200579E-16, 1.134196829589820086E-15 ) ) ;
#14029 = CIRCLE ( 'NONE', #14783, 0.5000000000000015543 ) ;
#14030 = CARTESIAN_POINT ( 'NONE',  ( 7.786490775660123376, -13.29349257805251305, 7.963863235126093620 ) ) ;
#14031 = AXIS2_PLACEMENT_3D ( 'NONE', #17394, #22585, #22477 ) ;
#14032 = CIRCLE ( 'NONE', #14405, 0.4999999999999998335 ) ;
#14033 = DIRECTION ( 'NONE',  ( -3.070652698126927723E-17, -1.000000000000000000, 4.167305704548413124E-17 ) ) ;
#14034 = LINE ( 'NONE', #23221, #17829 ) ;
#14035 = CARTESIAN_POINT ( 'NONE',  ( -55.05572809000119605, -3.200000000000088107, -7.500000000000062172 ) ) ;
#14036 = DIRECTION ( 'NONE',  ( 1.550910762415566494E-16, 1.000000000000000000, -8.135128085091684243E-31 ) ) ;
#14037 = DIRECTION ( 'NONE',  ( -1.000000000000000000, 1.550910762415566494E-16, -2.686847401719668638E-48 ) ) ;
#14038 = EDGE_CURVE ( 'NONE', #20382, #15390, #11646, .T. ) ;
#14039 = CARTESIAN_POINT ( 'NONE',  ( 4.346882592290811864, 1.739972214219157598, 1.970978495615613113 ) ) ;
#14040 = CARTESIAN_POINT ( 'NONE',  ( -7.955953741309951255, -12.35582749618196274, 7.654083333123914201 ) ) ;
#14041 = CARTESIAN_POINT ( 'NONE',  ( 12.49999999999997335, 1.500000000000015099, -9.500000000000001776 ) ) ;
#14042 = CARTESIAN_POINT ( 'NONE',  ( 108.2426266706970637, -13.52760560296359316, 5.999999999999984901 ) ) ;
#14043 = EDGE_LOOP ( 'NONE', ( #21005, #12769, #658, #12295 ) ) ;
#14044 = AXIS2_PLACEMENT_3D ( 'NONE', #4663, #13725, #2895 ) ;
#14045 = AXIS2_PLACEMENT_3D ( 'NONE', #7703, #12996, #13345 ) ;
#14047 = ORIENTED_EDGE ( 'NONE', *, *, #2682, .F. ) ;
#14046 = ORIENTED_EDGE ( 'NONE', *, *, #14900, .T. ) ;
#14048 = VECTOR ( 'NONE', #12928, 1000.000000000000000 ) ;
#14049 = ORIENTED_EDGE ( 'NONE', *, *, #12530, .T. ) ;
#14050 = VERTEX_POINT ( 'NONE', #5090 ) ;
#14051 = EDGE_LOOP ( 'NONE', ( #17037, #5548 ) ) ;
#14052 = ORIENTED_EDGE ( 'NONE', *, *, #15119, .F. ) ;
#14053 = EDGE_CURVE ( 'NONE', #4929, #6497, #773, .T. ) ;
#14054 = DIRECTION ( 'NONE',  ( 1.454462294001240516E-30, 1.000000000000000000, 0.000000000000000000 ) ) ;
#14055 = DIRECTION ( 'NONE',  ( 1.000000000000000000, 2.385244779468082934E-14, 0.000000000000000000 ) ) ;
#14056 = EDGE_LOOP ( 'NONE', ( #16921, #21146, #6012, #10512 ) ) ;
#14057 = DIRECTION ( 'NONE',  ( -1.000000000000000000, 4.190823558986610327E-31, -1.733449886265890494E-32 ) ) ;
#14058 = FACE_OUTER_BOUND ( 'NONE', #22121, .T. ) ;
#14059 = AXIS2_PLACEMENT_3D ( 'NONE', #18255, #14714, #15055 ) ;
#14060 = DIRECTION ( 'NONE',  ( 0.000000000000000000, -7.888609052210128564E-31, 1.000000000000000000 ) ) ;
#14061 = CLOSED_SHELL ( 'NONE', ( #8829, #11643, #9117, #17588, #9380, #18728, #10350, #8953, #14575, #3715, #1318, #9791, #9549, #4743, #4408, #5894, #14738, #4519, #5240, #1767, #4840, #6862, #11017, #13383, #21390, #3055, #8297, #11792, #19309, #16180, #2650, #3799, #11823, #23137, #15431, #3207, #8365, #12762, #10982, #17305, #7711, #17963, #1616, #11125, #7505, #14844, #17123, #4541, #3200, #19608, #9400, #4487, #22414, #19863, #19841, #7499, #11554, #16982, #18589, #20721, #22341, #13616, #12750, #8937, #14078, #15137, #13707, #11656, #2351, #5223, #9999, #13553, #10378, #6972, #6968, #7578, #3782, #13773, #7788, #549, #13137, #11102, #17381, #5649, #16296, #7487, #21149, #4604, #19592, #15707, #8407, #14865, #4610, #8140, #7919, #16530, #6415, #19595, #18602, #7382, #22678, #18434, #2267, #13717, #17206, #7945, #3052, #21630, #7883, #22488, #2482, #11413, #1313, #13290, #11953, #15680, #16239, #8134, #3653, #7227, #14137, #10446, #11355, #12698, #6513, #1180, #19368, #22078, #4918, #14007, #9691, #15906, #3024, #18356, #13982, #13833, #10399, #1123, #15269, #10740, #10325, #6378, #10684, #10510, #2468, #14426, #5807, #5311, #22453, #1059, #12120, #22158, #6478, #10697, #19629, #101, #21915, #10252, #6814, #9533, #2529, #21792, #4577, #3768, #10829, #15242 ) ) ;
#14062 = CIRCLE ( 'NONE', #9918, 0.4999999999999984457 ) ;
#14063 = CARTESIAN_POINT ( 'NONE',  ( -4.499999999708154341, 35.49999999900384751, -19.00000000000000355 ) ) ;
#14064 = DIRECTION ( 'NONE',  ( 0.000000000000000000, 0.000000000000000000, -1.000000000000000000 ) ) ;
#14065 = CARTESIAN_POINT ( 'NONE',  ( 29.00000000029184832, 16.99999999900385461, -15.99999999999999289 ) ) ;
#14066 = CIRCLE ( 'NONE', #20082, 6.000000000000000000 ) ;
#14067 = PLANE ( 'NONE',  #22782 ) ;
#14068 = SURFACE_STYLE_FILL_AREA ( #14184 ) ;
#14069 = DIRECTION ( 'NONE',  ( 0.000000000000000000, 0.000000000000000000, -1.000000000000000000 ) ) ;
#14070 = FACE_OUTER_BOUND ( 'NONE', #8316, .T. ) ;
#14071 = LINE ( 'NONE', #12290, #13396 ) ;
#14072 = SHAPE_REPRESENTATION ( 'Rubber Head', ( #22115 ), #20270 ) ;
#14073 = EDGE_LOOP ( 'NONE', ( #17249, #15647, #21262, #3086 ) ) ;
#14074 = CARTESIAN_POINT ( 'NONE',  ( 8.697224362267983011, -0.5000000000000004441, 6.250000000000061284 ) ) ;
#14075 = DIRECTION ( 'NONE',  ( 1.000000000000000000, 0.000000000000000000, 4.336808689941968432E-16 ) ) ;
#14077 = VERTEX_POINT ( 'NONE', #21094 ) ;
#14076 = ORIENTED_EDGE ( 'NONE', *, *, #10813, .T. ) ;
#14078 = ADVANCED_FACE ( 'NONE', ( #10376 ), #15554, .T. ) ;
#14079 = ORIENTED_EDGE ( 'NONE', *, *, #4167, .T. ) ;
#14080 = EDGE_LOOP ( 'NONE', ( #13129, #6186, #5791, #3939 ) ) ;
#14081 = ORIENTED_EDGE ( 'NONE', *, *, #5371, .F. ) ;
#14082 = CARTESIAN_POINT ( 'NONE',  ( 4.113620667976075396, 1.750000000000001554, -2.375000000000002220 ) ) ;
#14083 = DIRECTION ( 'NONE',  ( -1.858632295689435609E-16, -1.000000000000000000, -2.999267978177796234E-32 ) ) ;
#14084 = CARTESIAN_POINT ( 'NONE',  ( -6.000000000000102141, 4.799999999999964295, 8.000000000000047962 ) ) ;
#14085 = DIRECTION ( 'NONE',  ( -1.000000000000000000, 0.000000000000000000, -3.330669073875427220E-16 ) ) ;
#14086 = PLANE ( 'NONE',  #22253 ) ;
#14087 = DIRECTION ( 'NONE',  ( 9.121204216617949000E-31, 1.000000000000000000, -6.982962677686261977E-15 ) ) ;
#14088 = CARTESIAN_POINT ( 'NONE',  ( 4.175813232069142344, 2.061359961916322980, 3.570380186727409200 ) ) ;
#14089 = CARTESIAN_POINT ( 'NONE',  ( -7.282868595548795732, -0.2617430505220332271, 8.010178330700856719 ) ) ;
#14090 = DIRECTION ( 'NONE',  ( 0.000000000000000000, 0.000000000000000000, -1.000000000000000000 ) ) ;
#14091 = DIRECTION ( 'NONE',  ( -0.000000000000000000, 1.000000000000000000, -0.000000000000000000 ) ) ;
#14092 = VECTOR ( 'NONE', #19045, 1000.000000000000000 ) ;
#14093 = CYLINDRICAL_SURFACE ( 'NONE', #299, 0.4999999999999987232 ) ;
#14094 = B_SPLINE_CURVE_WITH_KNOTS ( 'NONE', 3,
 ( #411, #12994, #18514, #16387, #7355, #18402, #2048, #21599, #5476, #9232, #5937, #3701, #19821, #4152, #10871, #22049 ),
 .UNSPECIFIED., .F., .F.,
 ( 4, 3, 3, 3, 3, 4 ),
 ( -2.111273352554612095E-06, 0.000000000000000000, 3.519286887797705194E-05, 7.191842652069450729E-05, 0.0001049868727093782207, 0.0001382836236822282622 ),
 .UNSPECIFIED. ) ;
#14095 = CARTESIAN_POINT ( 'NONE',  ( 7.629227790279506927, -1.952801550923872309, 8.369856247450629283 ) ) ;
#14096 = FACE_OUTER_BOUND ( 'NONE', #8185, .T. ) ;
#14097 = CARTESIAN_POINT ( 'NONE',  ( -1.257172072276703467, 3.892973519170507934, -3.433252694550608553 ) ) ;
#14098 = EDGE_CURVE ( 'NONE', #4567, #4761, #15891, .T. ) ;
#14099 = CARTESIAN_POINT ( 'NONE',  ( -1.734723475976807094E-14, 2.000000000000001776, -17.00000000000000711 ) ) ;
#14100 = CARTESIAN_POINT ( 'NONE',  ( -1.655952806101454788, 3.662737355149022545, 2.873135757086587539E-15 ) ) ;
#14101 = ORIENTED_EDGE ( 'NONE', *, *, #7690, .T. ) ;
#14102 = EDGE_CURVE ( 'NONE', #14019, #6214, #19203, .T. ) ;
#14103 = ORIENTED_EDGE ( 'NONE', *, *, #15468, .T. ) ;
#14104 = CARTESIAN_POINT ( 'NONE',  ( -6.083292711281922394, 36.06725630338630140, -26.25729431478694664 ) ) ;
#14107 = ORIENTED_EDGE ( 'NONE', *, *, #23048, .T. ) ;
#14106 = ADVANCED_FACE ( 'NONE', ( #21224 ), #19430, .F. ) ;
#14105 = EDGE_LOOP ( 'NONE', ( #16598, #8755, #6677, #11548 ) ) ;
#14108 = AXIS2_PLACEMENT_3D ( 'NONE', #9047, #14465, #10807 ) ;
#14109 = EDGE_CURVE ( 'NONE', #9571, #18328, #9738, .T. ) ;
#14110 = CARTESIAN_POINT ( 'NONE',  ( -64.00000000000045475, 4.857225732735059864E-14, -1.999999999999974021 ) ) ;
#14111 = EDGE_CURVE ( 'NONE', #18843, #11516, #13910, .T. ) ;
#14112 = DIRECTION ( 'NONE',  ( -1.000000000000000000, -2.891205793294682764E-16, 0.000000000000000000 ) ) ;
#14113 = LINE ( 'NONE', #21297, #19364 ) ;
#14114 = DIRECTION ( 'NONE',  ( 2.013525853228507892E-32, 6.902532920683810383E-31, -1.000000000000000000 ) ) ;
#14115 = ORIENTED_EDGE ( 'NONE', *, *, #14703, .T. ) ;
#14116 = DIRECTION ( 'NONE',  ( 0.000000000000000000, -0.000000000000000000, -1.000000000000000000 ) ) ;
#14117 = CARTESIAN_POINT ( 'NONE',  ( -3.306986032670239384E-14, 0.6000000000000128564, -3.226721766443178208 ) ) ;
#14118 = CARTESIAN_POINT ( 'NONE',  ( 7.499999999999992895, -5.999999999999981348, 6.250000000000005329 ) ) ;
#14119 = LINE ( 'NONE', #15986, #15889 ) ;
#14120 = CARTESIAN_POINT ( 'NONE',  ( 0.3126073911696447549, -2.020725942163688504, 3.499999999999997780 ) ) ;
#14121 = CARTESIAN_POINT ( 'NONE',  ( 7.835522544085462116, -2.050824327339876074, 6.894286109559123688 ) ) ;
#14122 = CARTESIAN_POINT ( 'NONE',  ( 0.000000000000000000, 2.775557561562891351E-14, 17.49999999999997513 ) ) ;
#14123 = DIRECTION ( 'NONE',  ( 1.454462294001240516E-30, 1.000000000000000000, 0.000000000000000000 ) ) ;
#14124 = DIRECTION ( 'NONE',  ( -1.000000000000000000, -4.440892098500626162E-16, -5.551115123125782702E-16 ) ) ;
#14125 = ADVANCED_FACE ( 'NONE', ( #12137 ), #22940, .T. ) ;
#14126 = EDGE_CURVE ( 'NONE', #2880, #16146, #8856, .T. ) ;
#14127 = DIRECTION ( 'NONE',  ( 0.000000000000000000, 0.000000000000000000, -1.000000000000000000 ) ) ;
#14128 = SURFACE_SIDE_STYLE ('',( #22961 ) ) ;
#14129 = ORIENTED_EDGE ( 'NONE', *, *, #10223, .T. ) ;
#14130 = DIRECTION ( 'NONE',  ( 0.5804539248959941222, 0.8142930928559051207, -1.647731591911563963E-16 ) ) ;
#14132 = ORIENTED_EDGE ( 'NONE', *, *, #20728, .F. ) ;
#14131 = EDGE_LOOP ( 'NONE', ( #13559, #8084, #16143 ) ) ;
#14133 = ADVANCED_FACE ( 'NONE', ( #18137 ), #22012, .T. ) ;
#14134 = AXIS2_PLACEMENT_3D ( 'NONE', #17031, #15621, #4453 ) ;
#14135 = ORIENTED_EDGE ( 'NONE', *, *, #18995, .F. ) ;
#14138 = ORIENTED_EDGE ( 'NONE', *, *, #15256, .T. ) ;
#14137 = ADVANCED_FACE ( 'NONE', ( #257 ), #21567, .T. ) ;
#14136 = ORIENTED_EDGE ( 'NONE', *, *, #20885, .T. ) ;
#14139 = DIRECTION ( 'NONE',  ( -0.000000000000000000, -0.000000000000000000, 1.000000000000000000 ) ) ;
#14140 = EDGE_CURVE ( 'NONE', #13234, #9677, #4005, .T. ) ;
#14141 = LINE ( 'NONE', #21329, #23113 ) ;
#14142 = FACE_OUTER_BOUND ( 'NONE', #11750, .T. ) ;
#14143 = DIRECTION ( 'NONE',  ( 0.000000000000000000, 0.000000000000000000, 1.000000000000000000 ) ) ;
#14144 = DIRECTION ( 'NONE',  ( 1.000000000000000000, 3.254448077276381206E-32, 1.066788928082016908E-26 ) ) ;
#14145 = CARTESIAN_POINT ( 'NONE',  ( 119.5756419024615838, -6.500000000000005329, 6.000000000000158096 ) ) ;
#14146 = DIRECTION ( 'NONE',  ( 1.850371707708574881E-14, 0.000000000000000000, 1.000000000000000000 ) ) ;
#14147 = DIRECTION ( 'NONE',  ( -0.000000000000000000, 0.000000000000000000, -1.000000000000000000 ) ) ;
#14148 = DIRECTION ( 'NONE',  ( 0.000000000000000000, 0.000000000000000000, 1.000000000000000000 ) ) ;
#14149 = AXIS2_PLACEMENT_3D ( 'NONE', #6046, #13213, #13103 ) ;
#14150 = DIRECTION ( 'NONE',  ( -2.013525853228507892E-32, -6.902532920683810383E-31, 1.000000000000000000 ) ) ;
#14151 = CARTESIAN_POINT ( 'NONE',  ( 2.449848172108562316, 3.432307619358748951, -3.503702292528913187 ) ) ;
#14152 = DIRECTION ( 'NONE',  ( -9.121204216617949000E-31, -1.000000000000000000, 6.982962677686261977E-15 ) ) ;
#14153 = EDGE_CURVE ( 'NONE', #17539, #12680, #380, .T. ) ;
#14154 = CIRCLE ( 'NONE', #2114, 7.000000000000006217 ) ;
#14155 = DIRECTION ( 'NONE',  ( 1.000000000000000000, 0.000000000000000000, 0.000000000000000000 ) ) ;
#14156 = ADVANCED_FACE ( 'NONE', ( #5898 ), #4520, .T. ) ;
#14157 = AXIS2_PLACEMENT_3D ( 'NONE', #14644, #14183, #16390 ) ;
#14158 = DIRECTION ( 'NONE',  ( -1.331202777560457422E-30, -1.000000000000000000, 7.395570986446985676E-31 ) ) ;
#14159 = DIRECTION ( 'NONE',  ( -3.254448077146059901E-32, -1.000000000000000000, -6.409494854920712161E-31 ) ) ;
#14160 = ORIENTED_EDGE ( 'NONE', *, *, #16277, .T. ) ;
#14162 = ORIENTED_EDGE ( 'NONE', *, *, #4491, .F. ) ;
#14161 = VERTEX_POINT ( 'NONE', #1786 ) ;
#14163 = EDGE_CURVE ( 'NONE', #4569, #4546, #12408, .T. ) ;
#14164 = ORIENTED_EDGE ( 'NONE', *, *, #5386, .F. ) ;
#14165 = VECTOR ( 'NONE', #21223, 1000.000000000000000 ) ;
#14167 = EDGE_LOOP ( 'NONE', ( #11109, #4427, #20037, #8117 ) ) ;
#14166 = ORIENTED_EDGE ( 'NONE', *, *, #6144, .F. ) ;
#14168 = ORIENTED_EDGE ( 'NONE', *, *, #9391, .F. ) ;
#14169 = AXIS2_PLACEMENT_3D ( 'NONE', #13465, #22636, #11684 ) ;
#14170 = VERTEX_POINT ( 'NONE', #1891 ) ;
#14171 = CARTESIAN_POINT ( 'NONE',  ( -12.84999999999999964, -0.5000000000000004441, 0.000000000000000000 ) ) ;
#14172 = AXIS2_PLACEMENT_3D ( 'NONE', #13891, #1422, #11773 ) ;
#14173 = AXIS2_PLACEMENT_3D ( 'NONE', #4007, #16474, #2125 ) ;
#14174 = DIRECTION ( 'NONE',  ( 0.5000000000000025535, -0.8660254037844371533, 0.000000000000000000 ) ) ;
#14175 = VERTEX_POINT ( 'NONE', #9076 ) ;
#14176 = FACE_BOUND ( 'NONE', #13733, .T. ) ;
#14177 = CARTESIAN_POINT ( 'NONE',  ( 0.000000000000000000, 11.00000000000000000, -10.86602540378443749 ) ) ;
#14178 = VECTOR ( 'NONE', #7283, 1000.000000000000000 ) ;
#14179 = CARTESIAN_POINT ( 'NONE',  ( -12.85000000000002807, -13.50000000000003020, 6.250000000000033751 ) ) ;
#14180 = CARTESIAN_POINT ( 'NONE',  ( -4.499999999708154341, 36.49999999900384751, -19.00000000000000355 ) ) ;
#14181 = DIRECTION ( 'NONE',  ( 0.000000000000000000, 0.000000000000000000, 1.000000000000000000 ) ) ;
#14182 = DIRECTION ( 'NONE',  ( -1.454462294001240516E-30, -1.000000000000000000, -0.000000000000000000 ) ) ;
#14183 = DIRECTION ( 'NONE',  ( -0.6666666666666649643, -4.683861624749726065E-31, -0.7453559924999314523 ) ) ;
#14184 = FILL_AREA_STYLE ('',( #10300 ) ) ;
#14185 = CARTESIAN_POINT ( 'NONE',  ( 2.775557561562891351E-14, 10.99999999999998579, -3.000000000000002665 ) ) ;
#14186 = B_SPLINE_CURVE_WITH_KNOTS ( 'NONE', 3,
 ( #7156, #1387, #5387, #1837, #15609, #6680 ),
 .UNSPECIFIED., .F., .F.,
 ( 4, 2, 4 ),
 ( 0.007678960753836396383, 0.009067029700227515615, 0.01045509864661863311 ),
 .UNSPECIFIED. ) ;
#14187 = CARTESIAN_POINT ( 'NONE',  ( -4.182466315668081691, 13.41110669254460852, -15.99999999999999289 ) ) ;
#14188 = CARTESIAN_POINT ( 'NONE',  ( -8.495599073428085291, -1.515757017040946009, 7.013360899078306510 ) ) ;
#14189 = CIRCLE ( 'NONE', #22080, 2.500000000000015987 ) ;
#14190 = VERTEX_POINT ( 'NONE', #5558 ) ;
#14191 = EDGE_CURVE ( 'NONE', #3321, #13307, #19909, .T. ) ;
#14192 = DIRECTION ( 'NONE',  ( -1.000000000000000000, -0.000000000000000000, -1.613696256722611405E-16 ) ) ;
#14193 = DIRECTION ( 'NONE',  ( -1.550910762415566494E-16, -1.000000000000000000, 8.135128085091684243E-31 ) ) ;
#14195 = EDGE_LOOP ( 'NONE', ( #8844, #7407, #8271, #20650 ) ) ;
#14194 = ORIENTED_EDGE ( 'NONE', *, *, #18465, .T. ) ;
#14196 = VECTOR ( 'NONE', #7302, 1000.000000000000000 ) ;
#14197 = EDGE_CURVE ( 'NONE', #21322, #21919, #11283, .T. ) ;
#14198 = AXIS2_PLACEMENT_3D ( 'NONE', #21605, #5481, #12174 ) ;
#14199 = CIRCLE ( 'NONE', #14935, 2.099999999999999645 ) ;
#14200 = EDGE_LOOP ( 'NONE', ( #9592, #20278, #18413, #3051 ) ) ;
#14201 = VERTEX_POINT ( 'NONE', #16123 ) ;
#14202 = ORIENTED_EDGE ( 'NONE', *, *, #14851, .F. ) ;
#14203 = PRODUCT ( 'Handle Clip', 'Handle Clip', '', ( #14697 ) ) ;
#14204 = CONICAL_SURFACE ( 'NONE', #22464, 2.060000000000002718, 0.9599310885968758145 ) ;
#14205 = EDGE_CURVE ( 'NONE', #18123, #19164, #14662, .T. ) ;
#14206 = DIRECTION ( 'NONE',  ( 0.000000000000000000, 0.000000000000000000, 1.000000000000000000 ) ) ;
#14207 = AXIS2_PLACEMENT_3D ( 'NONE', #22196, #11476, #11354 ) ;
#14208 = CARTESIAN_POINT ( 'NONE',  ( 7.499999999999977796, -1.223704156646852281, 9.030675447288961877 ) ) ;
#14209 = CARTESIAN_POINT ( 'NONE',  ( 3.880206590543182177, 3.396506438958478480, -1.117078279489084558 ) ) ;
#14210 = CIRCLE ( 'NONE', #11938, 2.500000000000015987 ) ;
#14211 = CARTESIAN_POINT ( 'NONE',  ( 3.973514160553462737, 2.741076955031362949, 2.383932505289867887 ) ) ;
#14212 = CARTESIAN_POINT ( 'NONE',  ( -10.49999999999998224, -14.00000000000003020, 5.750000000000032863 ) ) ;
#14213 = LINE ( 'NONE', #15955, #20224 ) ;
#14214 = CARTESIAN_POINT ( 'NONE',  ( 6.000000000291855429, -9.961476088449217059E-10, -39.00000000000000000 ) ) ;
#14215 = FACE_OUTER_BOUND ( 'NONE', #21467, .T. ) ;
#14216 = CARTESIAN_POINT ( 'NONE',  ( -55.05572809000119605, -1.179611963664228824E-13, -8.000000000000090594 ) ) ;
#14217 = CYLINDRICAL_SURFACE ( 'NONE', #4412, 2.550000000000002043 ) ;
#14218 = CIRCLE ( 'NONE', #1036, 3.500000000000000000 ) ;
#14219 = LINE ( 'NONE', #14324, #8410 ) ;
#14220 = DIRECTION ( 'NONE',  ( 1.134196829589819889E-15, -1.111653967262545517E-30, 1.000000000000000000 ) ) ;
#14221 = CARTESIAN_POINT ( 'NONE',  ( -3.455068668935409093, 2.624017327438563640, -3.316620875264115753 ) ) ;
#14222 = CARTESIAN_POINT ( 'NONE',  ( -2.000000000000036415, 3.464101615137757495, 0.000000000000000000 ) ) ;
#14223 = EDGE_LOOP ( 'NONE', ( #13203, #4247, #21671, #1073 ) ) ;
#14224 = VECTOR ( 'NONE', #14957, 1000.000000000000000 ) ;
#14225 = VERTEX_POINT ( 'NONE', #21899 ) ;
#14226 = CARTESIAN_POINT ( 'NONE',  ( -4.690415759823429731, -0.7499999999999520384, -2.999999999999995559 ) ) ;
#14227 = VECTOR ( 'NONE', #3966, 1000.000000000000000 ) ;
#14229 = ORIENTED_EDGE ( 'NONE', *, *, #12754, .T. ) ;
#14228 = ORIENTED_EDGE ( 'NONE', *, *, #4213, .T. ) ;
#14230 = VECTOR ( 'NONE', #1957, 1000.000000000000000 ) ;
#14231 = CARTESIAN_POINT ( 'NONE',  ( 2.725741868436434068, -3.045094352033816953, -3.220599429844055894 ) ) ;
#14232 = DIRECTION ( 'NONE',  ( -4.003208021484906984E-16, 7.395570986447125806E-32, 1.000000000000000000 ) ) ;
#14233 = FACE_OUTER_BOUND ( 'NONE', #19010, .T. ) ;
#14234 = CARTESIAN_POINT ( 'NONE',  ( 5.600000000000000533, 0.000000000000000000, -3.469446951953614189E-15 ) ) ;
#14235 = CARTESIAN_POINT ( 'NONE',  ( 5.213674118230995802, 0.7500000000000561773, -1.500000000000001332 ) ) ;
#14236 = CARTESIAN_POINT ( 'NONE',  ( 0.000000000000000000, 0.5999999999999859890, -3.054668707061614086 ) ) ;
#14237 = B_SPLINE_CURVE_WITH_KNOTS ( 'NONE', 3,
 ( #22958, #10703, #17644, #5298 ),
 .UNSPECIFIED., .F., .F.,
 ( 4, 4 ),
 ( 0.002080789711329285828, 0.004173039763574515164 ),
 .UNSPECIFIED. ) ;
#14238 = LINE ( 'NONE', #1310, #22208 ) ;
#14239 = CARTESIAN_POINT ( 'NONE',  ( -7.835312244870005216, -13.94896639302768371, 7.041165740960562580 ) ) ;
#14240 = EDGE_CURVE ( 'NONE', #20477, #13207, #17287, .T. ) ;
#14241 = DIRECTION ( 'NONE',  ( -0.7071067811865462405, -2.274228861132049406E-16, -0.7071067811865489050 ) ) ;
#14242 = CARTESIAN_POINT ( 'NONE',  ( 8.260108127873506234, -2.109168607890740788, 7.249251683976269511 ) ) ;
#14243 = CARTESIAN_POINT ( 'NONE',  ( 3.999999999999955147, -2.309401076758532678, -3.433295621305388678 ) ) ;
#14244 = CARTESIAN_POINT ( 'NONE',  ( -3.999999999708139686, 13.32455531934060744, -15.99999999999999289 ) ) ;
#14245 = CARTESIAN_POINT ( 'NONE',  ( -3.649122391096853324, 1.701165921963302408, 3.179534615583007984 ) ) ;
#14246 = CIRCLE ( 'NONE', #19123, 3.999999999999999112 ) ;
#14247 = EDGE_CURVE ( 'NONE', #13411, #13010, #18372, .T. ) ;
#14248 = AXIS2_PLACEMENT_3D ( 'NONE', #19826, #3705, #5253 ) ;
#14249 = CARTESIAN_POINT ( 'NONE',  ( -61.45000000000046469, 3.200000000000057465, -1.999999999999973577 ) ) ;
#14250 = CARTESIAN_POINT ( 'NONE',  ( 4.175326769692856210, -4.121399112977853996, -4.789320010053836886E-15 ) ) ;
#14251 = ORIENTED_EDGE ( 'NONE', *, *, #16953, .T. ) ;
#14252 = PRODUCT_CONTEXT ( 'NONE', #12026, 'mechanical' ) ;
#14254 = ORIENTED_EDGE ( 'NONE', *, *, #20352, .F. ) ;
#14253 = ORIENTED_EDGE ( 'NONE', *, *, #17578, .T. ) ;
#14255 = ORIENTED_EDGE ( 'NONE', *, *, #8659, .F. ) ;
#14257 = EDGE_LOOP ( 'NONE', ( #17484, #10425, #12236, #10602, #14365, #21392, #4494 ) ) ;
#14256 = VERTEX_POINT ( 'NONE', #9198 ) ;
#14258 = CARTESIAN_POINT ( 'NONE',  ( 4.235886605889370493, 2.417314728048562067, -3.751161874094022686 ) ) ;
#14259 = DIRECTION ( 'NONE',  ( 1.000000000000000000, 0.000000000000000000, 0.000000000000000000 ) ) ;
#14260 = EDGE_CURVE ( 'NONE', #11952, #16292, #18055, .T. ) ;
#14261 = CARTESIAN_POINT ( 'NONE',  ( 7.500000000000007105, -11.35410196624971491, 9.250000000000014211 ) ) ;
#14262 = DIRECTION ( 'NONE',  ( -1.733449886265891589E-32, 4.190823558986610327E-31, -1.000000000000000000 ) ) ;
#14263 = FACE_OUTER_BOUND ( 'NONE', #31, .T. ) ;
#14264 = FACE_OUTER_BOUND ( 'NONE', #12535, .T. ) ;
#14265 = CARTESIAN_POINT ( 'NONE',  ( 4.690415759823637565, -0.7499999999999382716, -2.000000000000029310 ) ) ;
#14266 = ADVANCED_FACE ( 'NONE', ( #12835, #12604 ), #491, .T. ) ;
#14267 = CARTESIAN_POINT ( 'NONE',  ( -10.49999999999996803, -1.500000000000001332, 9.250000000000008882 ) ) ;
#14268 = CARTESIAN_POINT ( 'NONE',  ( 2.999999999999997335, -1.384721729257256131E-15, -4.749999999999984901 ) ) ;
#14269 = CARTESIAN_POINT ( 'NONE',  ( 1.660531772554329821, -3.660093687634886628, -2.145195642216240408E-14 ) ) ;
#14270 = CONICAL_SURFACE ( 'NONE', #4107, 4.000000000000022204, 0.8911886515913840512 ) ;
#14271 = CARTESIAN_POINT ( 'NONE',  ( -6.000000000000116351, 4.799999999999957190, -7.500000000000062172 ) ) ;
#14272 = CARTESIAN_POINT ( 'NONE',  ( 6.000000000291855429, 2.999999999003851503, -39.00000000000000000 ) ) ;
#14273 = DIRECTION ( 'NONE',  ( 0.000000000000000000, 0.000000000000000000, -1.000000000000000000 ) ) ;
#14274 = EDGE_CURVE ( 'NONE', #4090, #3970, #20016, .T. ) ;
#14275 = CARTESIAN_POINT ( 'NONE',  ( 88.75737332930596324, -6.527605602963476805, 6.000000000000165201 ) ) ;
#14276 = EDGE_CURVE ( 'NONE', #17281, #14364, #21056, .T. ) ;
#14277 = CARTESIAN_POINT ( 'NONE',  ( -6.000000000000116351, 1.999999999999960032, -7.500000000000062172 ) ) ;
#14278 = DIRECTION ( 'NONE',  ( -0.4999999999999999445, -4.767331059895059913E-16, -0.8660254037844387076 ) ) ;
#14279 = EDGE_CURVE ( 'NONE', #22552, #9468, #20256, .T. ) ;
#14280 = EDGE_LOOP ( 'NONE', ( #6125, #12231, #4868, #22405 ) ) ;
#14282 = ORIENTED_EDGE ( 'NONE', *, *, #13472, .F. ) ;
#14281 = ORIENTED_EDGE ( 'NONE', *, *, #17570, .F. ) ;
#14283 = EDGE_LOOP ( 'NONE', ( #13920, #13899, #4245 ) ) ;
#14285 = ORIENTED_EDGE ( 'NONE', *, *, #17277, .F. ) ;
#14284 = ORIENTED_EDGE ( 'NONE', *, *, #12685, .F. ) ;
#14286 = CIRCLE ( 'NONE', #22159, 2.550000000000010481 ) ;
#14287 = ORIENTED_EDGE ( 'NONE', *, *, #21934, .T. ) ;
#14288 = EDGE_CURVE ( 'NONE', #16175, #21212, #18801, .T. ) ;
#14289 = EDGE_LOOP ( 'NONE', ( #3246, #11085, #62, #8204 ) ) ;
#14290 = ORIENTED_EDGE ( 'NONE', *, *, #4306, .T. ) ;
#14291 = EDGE_CURVE ( 'NONE', #7030, #9040, #20705, .T. ) ;
#14292 = FACE_OUTER_BOUND ( 'NONE', #695, .T. ) ;
#14293 = ADVANCED_FACE ( 'NONE', ( #17050 ), #9892, .F. ) ;
#14294 = FACE_OUTER_BOUND ( 'NONE', #10804, .T. ) ;
#14295 = CARTESIAN_POINT ( 'NONE',  ( -7.500000000000034639, -12.77629584335315727, 9.030675447289006286 ) ) ;
#14296 = DIRECTION ( 'NONE',  ( -5.273559366969500667E-15, -6.938893903907237055E-15, -1.000000000000000000 ) ) ;
#14297 = DIRECTION ( 'NONE',  ( -2.013525853228508439E-32, -6.779273404243028164E-31, 1.000000000000000000 ) ) ;
#14298 = CARTESIAN_POINT ( 'NONE',  ( 3.806834918298653392, -3.031088913245548966, 1.749999999999996003 ) ) ;
#14299 = CARTESIAN_POINT ( 'NONE',  ( -4.154094228334058947, 2.398367420967200569, -3.721909803043219611 ) ) ;
#14300 = EDGE_CURVE ( 'NONE', #2718, #15424, #12795, .T. ) ;
#14301 =( NAMED_UNIT ( * ) SI_UNIT ( $, .STERADIAN. ) SOLID_ANGLE_UNIT ( ) );
#14302 = CARTESIAN_POINT ( 'NONE',  ( -4.690415759823443942, 0.7500000000000770495, -2.000000000000001776 ) ) ;
#14303 = EDGE_CURVE ( 'NONE', #3151, #18076, #8307, .T. ) ;
#14304 = DIRECTION ( 'NONE',  ( 0.000000000000000000, 0.000000000000000000, -1.000000000000000000 ) ) ;
#14305 = CARTESIAN_POINT ( 'NONE',  ( -8.391189084741213833, -1.526797151860788349, 7.111621047081270852 ) ) ;
#14306 = ORIENTED_EDGE ( 'NONE', *, *, #11403, .F. ) ;
#14307 =( NAMED_UNIT ( * ) PLANE_ANGLE_UNIT ( ) SI_UNIT ( $, .RADIAN. ) );
#14308 = CARTESIAN_POINT ( 'NONE',  ( -3.199999999999953104, -1.999999999999980904, -8.000000000000035527 ) ) ;
#14309 = CARTESIAN_POINT ( 'NONE',  ( -89.70000000000064233, 2.700000000000056577, -2.000000000000001776 ) ) ;
#14311 = VERTEX_POINT ( 'NONE', #20848 ) ;
#14310 = EDGE_LOOP ( 'NONE', ( #5521, #19188, #16630, #420 ) ) ;
#14312 = ORIENTED_EDGE ( 'NONE', *, *, #16659, .T. ) ;
#14313 = ORIENTED_EDGE ( 'NONE', *, *, #18177, .F. ) ;
#14314 = DIRECTION ( 'NONE',  ( 3.032184104443272185E-30, 1.000000000000000000, -7.395570986447005381E-32 ) ) ;
#14315 = CIRCLE ( 'NONE', #5675, 0.5000000000000004441 ) ;
#14316 = CARTESIAN_POINT ( 'NONE',  ( 3.999999999999989786, -2.309401076758549998, -0.3572655899081733644 ) ) ;
#14317 = CARTESIAN_POINT ( 'NONE',  ( 3.958484000407092029, 2.327740518748989906, -2.968235154690015865 ) ) ;
#14318 = DIRECTION ( 'NONE',  ( -0.7071067811865536790, 0.7071067811865413555, 0.000000000000000000 ) ) ;
#14319 = DIRECTION ( 'NONE',  ( -1.000000000000000000, -1.424116703980846297E-16, 1.095779650622964657E-32 ) ) ;
#14320 = CARTESIAN_POINT ( 'NONE',  ( 0.000000000000000000, 0.000000000000000000, 0.000000000000000000 ) ) ;
#14321 = CARTESIAN_POINT ( 'NONE',  ( 10.49999999999999467, -5.999999999999974243, 9.250000000000008882 ) ) ;
#14322 = DIRECTION ( 'NONE',  ( -6.656013887802287108E-31, -1.000000000000000000, 3.469446951953609061E-15 ) ) ;
#14323 = CARTESIAN_POINT ( 'NONE',  ( 37.42127086598691221, 10.78233971064650198, -10.42127086598680741 ) ) ;
#14324 = CARTESIAN_POINT ( 'NONE',  ( 58.04599508018838350, 2.194061104857452982, 6.000000000000095923 ) ) ;
#14325 = DIRECTION ( 'NONE',  ( 2.172745813409349776E-17, -1.000000000000000000, 1.309377075419428048E-16 ) ) ;
#14326 = CARTESIAN_POINT ( 'NONE',  ( -4.175648173966148846, 2.207990556236534729, -3.469390959564085719 ) ) ;
#14327 = EDGE_CURVE ( 'NONE', #2950, #11464, #22592, .T. ) ;
#14328 = DIRECTION ( 'NONE',  ( 3.330669073875432643E-16, 4.437342591868153746E-31, -1.000000000000000000 ) ) ;
#14330 = AXIS2_PLACEMENT_3D ( 'NONE', #1759, #17139, #15259 ) ;
#14329 = CARTESIAN_POINT ( 'NONE',  ( -0.3208286057740161734, 4.433571671609661813, -0.3503314178412331725 ) ) ;
#14331 = CIRCLE ( 'NONE', #15050, 0.4999999999999997224 ) ;
#14332 = ORIENTED_EDGE ( 'NONE', *, *, #4622, .T. ) ;
#14333 = EDGE_LOOP ( 'NONE', ( #3115, #14600, #4462, #447 ) ) ;
#14334 = CARTESIAN_POINT ( 'NONE',  ( -57.28378781035996070, 9.020562075079396891E-14, 8.541666666666724694 ) ) ;
#14335 = VERTEX_POINT ( 'NONE', #8126 ) ;
#14336 = APPLICATION_CONTEXT ( 'automotive_design' ) ;
#14337 = CARTESIAN_POINT ( 'NONE',  ( 5.600000000000000533, 2.020725942163695166, -3.500000000000034195 ) ) ;
#14338 = DIRECTION ( 'NONE',  ( 2.013525853228507892E-32, 6.902532920683810383E-31, -1.000000000000000000 ) ) ;
#14339 = CARTESIAN_POINT ( 'NONE',  ( 7.491585531133591047, -11.85620892266378235, 7.320610673787135703 ) ) ;
#14340 = ORIENTED_EDGE ( 'NONE', *, *, #3740, .F. ) ;
#14341 = DIRECTION ( 'NONE',  ( -1.000000000000000000, 1.550910762415566494E-16, 6.133276141584333908E-48 ) ) ;
#14342 = CIRCLE ( 'NONE', #12074, 9.500000000000056843 ) ;
#14343 = VECTOR ( 'NONE', #936, 1000.000000000000000 ) ;
#14344 = CYLINDRICAL_SURFACE ( 'NONE', #16798, 7.000000000000075495 ) ;
#14345 = DIRECTION ( 'NONE',  ( -1.000000000000000000, -1.479114197289397135E-31, -5.916456789157588541E-31 ) ) ;
#14346 = CARTESIAN_POINT ( 'NONE',  ( 4.000000000000003553, -1.933795701539624101, -0.2488376576623034797 ) ) ;
#14347 = FACE_OUTER_BOUND ( 'NONE', #17090, .T. ) ;
#14348 = CARTESIAN_POINT ( 'NONE',  ( -12.84999999999999964, -13.50000000000003020, 5.750000000000032863 ) ) ;
#14349 = DIRECTION ( 'NONE',  ( 2.013525853228507892E-32, 6.902532920683810383E-31, -1.000000000000000000 ) ) ;
#14350 = CARTESIAN_POINT ( 'NONE',  ( 0.000000000000000000, 0.000000000000000000, 0.000000000000000000 ) ) ;
#14351 = CARTESIAN_POINT ( 'NONE',  ( -2.742413778650712342, 1.325747111984031834, 4.749999999999999112 ) ) ;
#14352 = CIRCLE ( 'NONE', #842, 0.5000000000000017764 ) ;
#14353 = EDGE_CURVE ( 'NONE', #16829, #4291, #20719, .T. ) ;
#14354 = PLANE ( 'NONE',  #5568 ) ;
#14355 = ORIENTED_EDGE ( 'NONE', *, *, #8889, .F. ) ;
#14356 = APPLICATION_PROTOCOL_DEFINITION ( 'draft international standard', 'automotive_design', 1998, #17494 ) ;
#14357 = AXIS2_PLACEMENT_3D ( 'NONE', #8911, #5269, #16182 ) ;
#14359 = ORIENTED_EDGE ( 'NONE', *, *, #1659, .F. ) ;
#14358 = VERTEX_POINT ( 'NONE', #4581 ) ;
#14360 = VECTOR ( 'NONE', #3951, 1000.000000000000000 ) ;
#14361 = AXIS2_PLACEMENT_3D ( 'NONE', #1390, #21156, #23038 ) ;
#14362 = EDGE_CURVE ( 'NONE', #18328, #6218, #7913, .T. ) ;
#14363 = ORIENTED_EDGE ( 'NONE', *, *, #17473, .T. ) ;
#14365 = ORIENTED_EDGE ( 'NONE', *, *, #3421, .F. ) ;
#14364 = VERTEX_POINT ( 'NONE', #15289 ) ;
#14366 = CYLINDRICAL_SURFACE ( 'NONE', #10265, 2.550000000000010481 ) ;
#14367 = DIRECTION ( 'NONE',  ( 0.000000000000000000, 4.336808689941991704E-15, 1.000000000000000000 ) ) ;
#14368 = CARTESIAN_POINT ( 'NONE',  ( 7.500000000000008882, -10.98142396999974224, 8.916666666666674956 ) ) ;
#14369 = VECTOR ( 'NONE', #845, 1000.000000000000000 ) ;
#14370 = DIRECTION ( 'NONE',  ( 0.000000000000000000, 1.000000000000000000, 0.000000000000000000 ) ) ;
#14371 = CARTESIAN_POINT ( 'NONE',  ( 10.50000000000000888, -1.500000000000001332, 9.250000000000008882 ) ) ;
#14372 = CARTESIAN_POINT ( 'NONE',  ( 12.84999999999997300, -12.50000000000006928, 5.551115123125782702E-14 ) ) ;
#14373 = CARTESIAN_POINT ( 'NONE',  ( -50.65685424949281668, 2.700000000000021938, 7.500000000000034639 ) ) ;
#14374 = CARTESIAN_POINT ( 'NONE',  ( 2.775557561562891351E-14, 2.499999999999998668, -6.499999999999950262 ) ) ;
#14375 = CARTESIAN_POINT ( 'NONE',  ( -65.00000000000044054, -3.200000000000088107, 2.999999999999947153 ) ) ;
#14376 = CIRCLE ( 'NONE', #10975, 0.5000000000000022204 ) ;
#14377 = FACE_OUTER_BOUND ( 'NONE', #11311, .T. ) ;
#14378 = CIRCLE ( 'NONE', #17373, 0.2500000000000003331 ) ;
#14379 = CYLINDRICAL_SURFACE ( 'NONE', #4978, 0.4999999999999978351 ) ;
#14380 = VECTOR ( 'NONE', #12517, 1000.000000000000000 ) ;
#14381 = AXIS2_PLACEMENT_3D ( 'NONE', #6914, #17607, #21033 ) ;
#14382 = DIRECTION ( 'NONE',  ( -1.000000000000000000, 1.550910762415469612E-16, 0.000000000000000000 ) ) ;
#14383 = DIRECTION ( 'NONE',  ( 3.885780586188016830E-16, 4.437342591868156373E-31, -1.000000000000000000 ) ) ;
#14384 = B_SPLINE_CURVE_WITH_KNOTS ( 'NONE', 3,
 ( #5326, #14269, #23107, #21098, #4964, #12485 ),
 .UNSPECIFIED., .F., .F.,
 ( 4, 2, 4 ),
 ( 0.002336974151641521731, 0.003500975885716451057, 0.004664977619791380384 ),
 .UNSPECIFIED. ) ;
#14385 = CARTESIAN_POINT ( 'NONE',  ( -4.550510256924974684, 35.99999999900384751, -19.50000000000000355 ) ) ;
#14386 = CARTESIAN_POINT ( 'NONE',  ( 5.600000000000000533, 3.061616997868409765E-16, -2.500000000000003997 ) ) ;
#14387 = ORIENTED_EDGE ( 'NONE', *, *, #21666, .F. ) ;
#14388 = EDGE_CURVE ( 'NONE', #20542, #18441, #727, .T. ) ;
#14389 = SURFACE_SIDE_STYLE ('',( #6873 ) ) ;
#14391 = ORIENTED_EDGE ( 'NONE', *, *, #14656, .F. ) ;
#14390 = ORIENTED_EDGE ( 'NONE', *, *, #19414, .F. ) ;
#14392 = EDGE_CURVE ( 'NONE', #18197, #7574, #16916, .T. ) ;
#14393 = ORIENTED_EDGE ( 'NONE', *, *, #9415, .T. ) ;
#14394 = AXIS2_PLACEMENT_3D ( 'NONE', #21376, #17835, #18184 ) ;
#14395 = VECTOR ( 'NONE', #6482, 1000.000000000000000 ) ;
#14397 = VERTEX_POINT ( 'NONE', #16807 ) ;
#14396 = EDGE_LOOP ( 'NONE', ( #8869, #14905, #5545, #22092 ) ) ;
#14398 = AXIS2_PLACEMENT_3D ( 'NONE', #12725, #23105, #17799 ) ;
#14399 = ORIENTED_EDGE ( 'NONE', *, *, #19207, .F. ) ;
#14400 = VECTOR ( 'NONE', #2651, 1000.000000000000000 ) ;
#14401 = CIRCLE ( 'NONE', #137, 0.4999999999999994449 ) ;
#14402 = VERTEX_POINT ( 'NONE', #837 ) ;
#14403 = AXIS2_PLACEMENT_3D ( 'NONE', #19667, #6981, #18131 ) ;
#14404 = EDGE_LOOP ( 'NONE', ( #4917, #4751, #7904, #9981 ) ) ;
#14405 = AXIS2_PLACEMENT_3D ( 'NONE', #17791, #20976, #12365 ) ;
#14406 = CARTESIAN_POINT ( 'NONE',  ( -95.70000000000069917, 2.700000000000014833, -2.000000000000001776 ) ) ;
#14407 = EDGE_CURVE ( 'NONE', #22641, #7652, #4344, .T. ) ;
#14408 = EDGE_CURVE ( 'NONE', #9471, #20563, #12046, .T. ) ;
#14409 = DIRECTION ( 'NONE',  ( 2.013525853228507892E-32, 6.902532920683810383E-31, -1.000000000000000000 ) ) ;
#14410 = DIRECTION ( 'NONE',  ( -1.000000000000000000, 1.550910762415566494E-16, -2.686847401719668638E-48 ) ) ;
#14411 = EDGE_CURVE ( 'NONE', #21027, #20477, #4535, .T. ) ;
#14412 = CARTESIAN_POINT ( 'NONE',  ( -4.499999999708154341, 36.49999999900384751, -25.50000000000000000 ) ) ;
#14413 = CARTESIAN_POINT ( 'NONE',  ( 1.448045174978588829E-14, 2.859595677584339857, -2.047034997319622018 ) ) ;
#14414 = CARTESIAN_POINT ( 'NONE',  ( 73.50000000000112266, -3.999999999999809042, 1.179611963664228824E-13 ) ) ;
#14415 = CARTESIAN_POINT ( 'NONE',  ( 4.690415759823373776, -0.7499999999999382716, -1.500000000000001332 ) ) ;
#14416 = PLANE ( 'NONE',  #14198 ) ;
#14417 = AXIS2_PLACEMENT_3D ( 'NONE', #11020, #14667, #439 ) ;
#14418 = CIRCLE ( 'NONE', #10276, 0.4999999999999978351 ) ;
#14419 = CARTESIAN_POINT ( 'NONE',  ( 2.889332061078579539, 4.882140790251119356, 7.500000000000007105 ) ) ;
#14420 = CIRCLE ( 'NONE', #4255, 0.5000000000000029976 ) ;
#14421 = DIRECTION ( 'NONE',  ( 3.254448077146059901E-32, 1.000000000000000000, 6.409494854920712161E-31 ) ) ;
#14422 = ADVANCED_FACE ( 'NONE', ( #22127 ), #6018, .T. ) ;
#14423 = ORIENTED_EDGE ( 'NONE', *, *, #23086, .F. ) ;
#14424 = AXIS2_PLACEMENT_3D ( 'NONE', #18566, #2217, #16326 ) ;
#14425 = EDGE_CURVE ( 'NONE', #4929, #17843, #15052, .T. ) ;
#14426 = ADVANCED_FACE ( 'NONE', ( #2703 ), #6132, .T. ) ;
#14427 = DIRECTION ( 'NONE',  ( 0.000000000000000000, 1.000000000000000000, 0.000000000000000000 ) ) ;
#14429 = ORIENTED_EDGE ( 'NONE', *, *, #22600, .T. ) ;
#14428 = ORIENTED_EDGE ( 'NONE', *, *, #17610, .T. ) ;
#14430 = VERTEX_POINT ( 'NONE', #8246 ) ;
#14432 = ORIENTED_EDGE ( 'NONE', *, *, #7491, .F. ) ;
#14431 = EDGE_CURVE ( 'NONE', #6724, #16375, #18477, .T. ) ;
#14433 = PLANE ( 'NONE',  #3176 ) ;
#14434 = CIRCLE ( 'NONE', #12916, 4.500000000000000888 ) ;
#14435 = ADVANCED_FACE ( 'NONE', ( #6714 ), #10128, .T. ) ;
#14436 = AXIS2_PLACEMENT_3D ( 'NONE', #16045, #9234, #23254 ) ;
#14437 = CARTESIAN_POINT ( 'NONE',  ( 0.000000000000000000, 1.387778780781445676E-14, -25.03750572909315508 ) ) ;
#14438 = CARTESIAN_POINT ( 'NONE',  ( -4.113620667976075396, 1.749999999999998002, 2.374999999999998668 ) ) ;
#14439 = EDGE_CURVE ( 'NONE', #16514, #10173, #3420, .T. ) ;
#14440 = CARTESIAN_POINT ( 'NONE',  ( 4.175813232069149450, -2.061359961916378492, -3.570380186727402538 ) ) ;
#14441 = CARTESIAN_POINT ( 'NONE',  ( 6.500000000000005329, 1.665334536937734811E-13, 3.469446951953614189E-14 ) ) ;
#14442 = CARTESIAN_POINT ( 'NONE',  ( -55.05572809000125289, 1.387778780781445676E-14, -10.00000000000006395 ) ) ;
#14443 = EDGE_CURVE ( 'NONE', #9710, #17392, #11294, .T. ) ;
#14444 = B_SPLINE_CURVE_WITH_KNOTS ( 'NONE', 3,
 ( #4098, #584, #6108, #11734, #15153, #18681, #5997, #16906, #9631, #4322 ),
 .UNSPECIFIED., .F., .F.,
 ( 4, 2, 2, 2, 4 ),
 ( 0.001114109625932955920, 0.001508381724359308257, 0.001902653822785660810, 0.002296925921212013364, 0.002691198019638365701 ),
 .UNSPECIFIED. ) ;
#14445 = CARTESIAN_POINT ( 'NONE',  ( 88.75737332930592061, -6.527605602963476805, -6.000000000000012434 ) ) ;
#14446 = CARTESIAN_POINT ( 'NONE',  ( 0.000000000000000000, -1.750000000000001554, 0.000000000000000000 ) ) ;
#14447 = CARTESIAN_POINT ( 'NONE',  ( 86.02937988905580369, -9.453020409440155092, -6.499999999999943157 ) ) ;
#14448 = CARTESIAN_POINT ( 'NONE',  ( 37.51717533640845659, 10.97664592903658232, -10.69160037009666020 ) ) ;
#14449 = CARTESIAN_POINT ( 'NONE',  ( 119.5756419024615411, -7.000000000000006217, 6.000000000000095923 ) ) ;
#14450 = CARTESIAN_POINT ( 'NONE',  ( 2.775557561562891351E-14, 2.999999999999999112, -12.99999999999999822 ) ) ;
#14451 = DIRECTION ( 'NONE',  ( -1.134196829589822059E-15, -6.741645191078037727E-32, 1.000000000000000000 ) ) ;
#14452 = TOROIDAL_SURFACE ( 'NONE', #6563, 3.500000000000000000, 0.5000000000000000000 ) ;
#14453 = CARTESIAN_POINT ( 'NONE',  ( 27.99999999999991473, -3.469446951953614189E-15, -2.775557561562891351E-14 ) ) ;
#14454 = AXIS2_PLACEMENT_3D ( 'NONE', #9684, #13682, #2730 ) ;
#14455 = AXIS2_PLACEMENT_3D ( 'NONE', #6139, #9319, #20024 ) ;
#14456 = CARTESIAN_POINT ( 'NONE',  ( 10.49999999999999467, -8.000000000000031974, 9.250000000000021316 ) ) ;
#14457 = VERTEX_POINT ( 'NONE', #8591 ) ;
#14458 = AXIS2_PLACEMENT_3D ( 'NONE', #22270, #2856, #637 ) ;
#14459 = ORIENTED_EDGE ( 'NONE', *, *, #9991, .T. ) ;
#14460 = EDGE_CURVE ( 'NONE', #16146, #22503, #16178, .T. ) ;
#14461 = CARTESIAN_POINT ( 'NONE',  ( -3.999999999708153453, 38.99999999900385461, -29.00000000000000355 ) ) ;
#14462 = ORIENTED_EDGE ( 'NONE', *, *, #10420, .T. ) ;
#14463 = CARTESIAN_POINT ( 'NONE',  ( 3.455068668934203391, -2.624017327439216896, -3.316620875263055712 ) ) ;
#14464 = CARTESIAN_POINT ( 'NONE',  ( 2.687328764639619116, -3.067272167851354592, -0.05923475698273424767 ) ) ;
#14465 = DIRECTION ( 'NONE',  ( 0.000000000000000000, -1.000000000000000000, 0.000000000000000000 ) ) ;
#14466 =( LENGTH_UNIT ( ) NAMED_UNIT ( * ) SI_UNIT ( .MILLI., .METRE. ) );
#14467 = CIRCLE ( 'NONE', #6950, 2.500000000000000000 ) ;
#14468 = ORIENTED_EDGE ( 'NONE', *, *, #1904, .F. ) ;
#14469 = DIRECTION ( 'NONE',  ( -1.000000000000000000, -2.220446049250314067E-16, 5.825996348268307008E-33 ) ) ;
#14470 = FACE_OUTER_BOUND ( 'NONE', #15746, .T. ) ;
#14471 = CARTESIAN_POINT ( 'NONE',  ( 26.45000000029184051, 16.99999999900385461, -29.00000000000000355 ) ) ;
#14472 = CARTESIAN_POINT ( 'NONE',  ( -6.999999999999993783, -13.21292803502077184, 9.239863038076370216 ) ) ;
#14473 = DIRECTION ( 'NONE',  ( -1.000000000000000000, 2.168404344970992105E-16, -8.673617379883968419E-16 ) ) ;
#14474 = PLANE ( 'NONE',  #1785 ) ;
#14475 = CARTESIAN_POINT ( 'NONE',  ( 4.211140560182194292, -2.431303136016568889, -3.745885042887441063 ) ) ;
#14476 = CARTESIAN_POINT ( 'NONE',  ( 3.974175853610087739, -3.450041667725798344, 1.156004144284031199 ) ) ;
#14477 = DIRECTION ( 'NONE',  ( 2.220446049250313081E-16, -1.000000000000000000, 7.025792437124636392E-31 ) ) ;
#14478 = DIRECTION ( 'NONE',  ( -1.000000000000000000, -2.220446049250314067E-16, 5.825996348268307008E-33 ) ) ;
#14479 = B_SPLINE_CURVE_WITH_KNOTS ( 'NONE', 3,
 ( #20389, #7572, #520, #11553 ),
 .UNSPECIFIED., .F., .F.,
 ( 4, 4 ),
 ( 2.380739282131849795E-07, 0.002044882221487523237 ),
 .UNSPECIFIED. ) ;
#14480 = ORIENTED_EDGE ( 'NONE', *, *, #17393, .F. ) ;
#14481 = SHAPE_DEFINITION_REPRESENTATION ( #19064, #11650 ) ;
#14482 = VECTOR ( 'NONE', #1529, 1000.000000000000000 ) ;
#14484 = VERTEX_POINT ( 'NONE', #8479 ) ;
#14483 = ORIENTED_EDGE ( 'NONE', *, *, #13179, .T. ) ;
#14485 = EDGE_CURVE ( 'NONE', #2116, #9302, #11663, .T. ) ;
#14487 = EDGE_LOOP ( 'NONE', ( #251, #4168, #4639, #10251 ) ) ;
#14486 = ORIENTED_EDGE ( 'NONE', *, *, #5634, .F. ) ;
#14488 = DIRECTION ( 'NONE',  ( -1.000000000000000000, -2.220446049250301001E-16, 0.000000000000000000 ) ) ;
#14489 = EDGE_CURVE ( 'NONE', #9370, #20776, #15758, .T. ) ;
#14490 = CARTESIAN_POINT ( 'NONE',  ( 0.000000000000000000, 1.750000000000001554, 0.000000000000000000 ) ) ;
#14491 = AXIS2_PLACEMENT_3D ( 'NONE', #14446, #18316, #5624 ) ;
#14492 = CARTESIAN_POINT ( 'NONE',  ( -8.565230440156030411, -12.00000000000004441, 6.320505311736962284 ) ) ;
#14493 = CARTESIAN_POINT ( 'NONE',  ( 0.000000000000000000, 0.000000000000000000, 0.000000000000000000 ) ) ;
#14494 = DIRECTION ( 'NONE',  ( -9.121204216617949000E-31, -1.000000000000000000, 6.982962677686261977E-15 ) ) ;
#14495 =( NAMED_UNIT ( * ) SI_UNIT ( $, .STERADIAN. ) SOLID_ANGLE_UNIT ( ) );
#14496 = DIRECTION ( 'NONE',  ( -2.013525853228507892E-32, -6.902532920683810383E-31, 1.000000000000000000 ) ) ;
#14497 = CARTESIAN_POINT ( 'NONE',  ( 113.0166151911345906, -11.64708151429785765, 6.000000000000067502 ) ) ;
#14498 = CARTESIAN_POINT ( 'NONE',  ( -8.697224362268011433, -1.499999999999984013, 6.250000000000005329 ) ) ;
#14499 = FACE_OUTER_BOUND ( 'NONE', #17569, .T. ) ;
#14500 = ADVANCED_FACE ( 'NONE', ( #17763 ), #22956, .F. ) ;
#14501 = CARTESIAN_POINT ( 'NONE',  ( -2.081668171172168513E-14, 2.000000000000001776, -0.2500000000000002220 ) ) ;
#14502 = CARTESIAN_POINT ( 'NONE',  ( 73.50000000000116529, -13.52760560296348302, -2.549999999999978062 ) ) ;
#14503 = ORIENTED_EDGE ( 'NONE', *, *, #1339, .T. ) ;
#14504 = FILL_AREA_STYLE_COLOUR ( '', #4110 ) ;
#14506 = VERTEX_POINT ( 'NONE', #8355 ) ;
#14505 = ORIENTED_EDGE ( 'NONE', *, *, #8411, .F. ) ;
#14507 = ORIENTED_EDGE ( 'NONE', *, *, #2349, .F. ) ;
#14509 = ORIENTED_EDGE ( 'NONE', *, *, #12592, .T. ) ;
#14508 = EDGE_LOOP ( 'NONE', ( #14731, #19166, #16797 ) ) ;
#14510 = AXIS2_PLACEMENT_3D ( 'NONE', #8915, #20087, #19965 ) ;
#14511 = ORIENTED_EDGE ( 'NONE', *, *, #20482, .F. ) ;
#14512 = CARTESIAN_POINT ( 'NONE',  ( 4.132952817037863547, 2.031684012687259955, 3.518979934899744588 ) ) ;
#14513 = ORIENTED_EDGE ( 'NONE', *, *, #18875, .F. ) ;
#14514 = EDGE_LOOP ( 'NONE', ( #15241, #6223, #22995, #19642, #3802, #13086 ) ) ;
#14515 = CARTESIAN_POINT ( 'NONE',  ( 0.8691243128804460039, 0.6000000000000137446, 4.444585127983383899 ) ) ;
#14516 = DIRECTION ( 'NONE',  ( -1.000000000000000000, 0.000000000000000000, 0.000000000000000000 ) ) ;
#14517 = DIRECTION ( 'NONE',  ( 1.000000000000000000, -0.000000000000000000, 0.000000000000000000 ) ) ;
#14518 = VECTOR ( 'NONE', #17238, 1000.000000000000000 ) ;
#14519 = PRODUCT_DEFINITION ( 'UNKNOWN', '', #10138, #18521 ) ;
#14520 = DIRECTION ( 'NONE',  ( -0.9706398123736329486, -2.155253336630096955E-16, -0.2405376366294442458 ) ) ;
#14521 = DIRECTION ( 'NONE',  ( 1.000000000000000000, -1.858632295689435609E-16, 0.000000000000000000 ) ) ;
#14522 = CARTESIAN_POINT ( 'NONE',  ( -4.197393957002393705, 0.4069871074557405710, -3.503767560748956011 ) ) ;
#14523 = ADVANCED_FACE ( 'NONE', ( #5179 ), #7072, .T. ) ;
#14524 = DIRECTION ( 'NONE',  ( 1.333893503340774882E-15, 2.778352770573747380E-17, 1.000000000000000000 ) ) ;
#14525 = CARTESIAN_POINT ( 'NONE',  ( 124.5000000000019185, -6.500000000000005329, 6.500000000000214051 ) ) ;
#14526 = CARTESIAN_POINT ( 'NONE',  ( 37.57823792062858104, 10.91119608832008581, -2.709549562527672872 ) ) ;
#14527 = EDGE_LOOP ( 'NONE', ( #2499, #20533, #5347, #7827, #1809, #3581 ) ) ;
#14528 = EDGE_CURVE ( 'NONE', #12123, #21498, #19291, .T. ) ;
#14529 = CARTESIAN_POINT ( 'NONE',  ( 2.775557561562891351E-14, 8.000000000000003553, -15.49999999999998579 ) ) ;
#14531 = ORIENTED_EDGE ( 'NONE', *, *, #1979, .F. ) ;
#14530 = VERTEX_POINT ( 'NONE', #10473 ) ;
#14532 = EDGE_CURVE ( 'NONE', #5983, #555, #14315, .T. ) ;
#14533 = AXIS2_PLACEMENT_3D ( 'NONE', #20269, #14618, #10958 ) ;
#14534 = ORIENTED_EDGE ( 'NONE', *, *, #1347, .T. ) ;
#14535 = ORIENTED_EDGE ( 'NONE', *, *, #22905, .T. ) ;
#14536 = ORIENTED_EDGE ( 'NONE', *, *, #11696, .F. ) ;
#14537 = ORIENTED_EDGE ( 'NONE', *, *, #18861, .F. ) ;
#14538 = LINE ( 'NONE', #94, #15912 ) ;
#14539 = DIRECTION ( 'NONE',  ( -2.172745813409349776E-17, 1.000000000000000000, -1.309377075419428048E-16 ) ) ;
#14540 = CARTESIAN_POINT ( 'NONE',  ( -45.56568542494948559, -2.108831175456959972, 7.500000000000076383 ) ) ;
#14541 = EDGE_CURVE ( 'NONE', #12036, #10173, #9056, .T. ) ;
#14542 = CARTESIAN_POINT ( 'NONE',  ( 24.75000000000002487, 1.250000000000001110, -2.000000000000005329 ) ) ;
#14543 = DIRECTION ( 'NONE',  ( 1.000000000000000000, 0.000000000000000000, 4.336808689941968432E-16 ) ) ;
#14544 = AXIS2_PLACEMENT_3D ( 'NONE', #5537, #21545, #3424 ) ;
#14545 = CARTESIAN_POINT ( 'NONE',  ( 8.495599073428115489, -12.48424298295908130, 7.013360899078397992 ) ) ;
#14546 = DIRECTION ( 'NONE',  ( -1.000000000000000000, 1.550910762415526064E-16, 0.000000000000000000 ) ) ;
#14547 = AXIS2_PLACEMENT_3D ( 'NONE', #5980, #13152, #4185 ) ;
#14548 = ADVANCED_FACE ( 'NONE', ( #17521 ), #57, .T. ) ;
#14549 = FACE_OUTER_BOUND ( 'NONE', #16228, .T. ) ;
#14550 = CARTESIAN_POINT ( 'NONE',  ( 37.34641016151397963, 10.60000000000007425, -10.34641016151376824 ) ) ;
#14551 = DIRECTION ( 'NONE',  ( 9.121204216617949000E-31, 1.000000000000000000, -6.982962677686261977E-15 ) ) ;
#14552 = DIRECTION ( 'NONE',  ( 2.220446049250313081E-16, -1.000000000000000000, 7.025792437124636392E-31 ) ) ;
#14553 = CARTESIAN_POINT ( 'NONE',  ( 124.5000000000019469, -13.52760560296373171, 2.550000000000006040 ) ) ;
#14554 = CIRCLE ( 'NONE', #22847, 3.499999999999995115 ) ;
#14555 = EDGE_CURVE ( 'NONE', #1883, #21928, #14238, .T. ) ;
#14556 = FACE_OUTER_BOUND ( 'NONE', #11061, .T. ) ;
#14557 = CARTESIAN_POINT ( 'NONE',  ( 37.00000000000014211, 11.00000000000000000, -3.000000000000002665 ) ) ;
#14558 = EDGE_CURVE ( 'NONE', #13358, #19695, #4158, .T. ) ;
#14559 = EDGE_LOOP ( 'NONE', ( #20511, #11034 ) ) ;
#14560 = ORIENTED_EDGE ( 'NONE', *, *, #17416, .T. ) ;
#14561 = CIRCLE ( 'NONE', #7079, 3.300000000000020250 ) ;
#14562 = CIRCLE ( 'NONE', #10440, 7.499999999999998224 ) ;
#14563 = CARTESIAN_POINT ( 'NONE',  ( -50.65685424949267457, -3.200000000000108979, -7.500000000000034639 ) ) ;
#14564 = DIRECTION ( 'NONE',  ( -0.7071067811865580088, -0.7071067811865372477, 0.000000000000000000 ) ) ;
#14565 = ORIENTED_EDGE ( 'NONE', *, *, #20189, .F. ) ;
#14566 = CIRCLE ( 'NONE', #2156, 2.999999999999995559 ) ;
#14567 = ADVANCED_FACE ( 'NONE', ( #5063 ), #8708, .T. ) ;
#14568 = CARTESIAN_POINT ( 'NONE',  ( -12.84999999999999964, -2.011595308313580664E-30, 2.549999999999997158 ) ) ;
#14569 = CARTESIAN_POINT ( 'NONE',  ( -2.000000000000015543, -3.464101615137743728, -5.600000000000000533 ) ) ;
#14570 = EDGE_CURVE ( 'NONE', #19198, #6388, #1284, .T. ) ;
#14571 = DIRECTION ( 'NONE',  ( -1.000000000000000000, -5.598259082250514647E-17, -3.330669073875432643E-16 ) ) ;
#14572 = CARTESIAN_POINT ( 'NONE',  ( -50.65685424949274562, -7.200000000000077449, 8.000000000000062172 ) ) ;
#14573 = EDGE_CURVE ( 'NONE', #5312, #16601, #7546, .T. ) ;
#14574 = CIRCLE ( 'NONE', #1070, 0.5000000000000038858 ) ;
#14575 = ADVANCED_FACE ( 'NONE', ( #21541 ), #11043, .F. ) ;
#14576 = VERTEX_POINT ( 'NONE', #5534 ) ;
#14577 = DIRECTION ( 'NONE',  ( 3.032184104443272185E-30, 1.000000000000000000, -7.395570986447005381E-32 ) ) ;
#14578 = CARTESIAN_POINT ( 'NONE',  ( 1.110223024625156540E-13, -1.750000000000001554, -4.750000000000000888 ) ) ;
#14579 = AXIS2_PLACEMENT_3D ( 'NONE', #8190, #11705, #18895 ) ;
#14580 = DIRECTION ( 'NONE',  ( -4.336808689942045346E-15, 1.000000000000000000, 7.518830502887770522E-31 ) ) ;
#14581 = CARTESIAN_POINT ( 'NONE',  ( 7.168696526429616966, -13.62622308581068253, 8.340670630249162443 ) ) ;
#14582 = FACE_OUTER_BOUND ( 'NONE', #15422, .T. ) ;
#14583 = PLANE ( 'NONE',  #17171 ) ;
#14584 = FACE_OUTER_BOUND ( 'NONE', #16173, .T. ) ;
#14585 = DIRECTION ( 'NONE',  ( 0.000000000000000000, 0.000000000000000000, 1.000000000000000000 ) ) ;
#14586 = EDGE_CURVE ( 'NONE', #4671, #17191, #13922, .T. ) ;
#14587 = SURFACE_STYLE_USAGE ( .BOTH. , #7416 ) ;
#14588 = COLOUR_RGB ( '', 0.09019608, 0.27058824, 0.51372549) ;
#14589 = EDGE_CURVE ( 'NONE', #1642, #22215, #14687, .T. ) ;
#14590 = CYLINDRICAL_SURFACE ( 'NONE', #16074, 2.550000000000010481 ) ;
#14591 = AXIS2_PLACEMENT_3D ( 'NONE', #13963, #16184, #5148 ) ;
#14592 = EDGE_CURVE ( 'NONE', #5384, #477, #5424, .T. ) ;
#14593 = AXIS2_PLACEMENT_3D ( 'NONE', #16656, #14903, #22089 ) ;
#14594 = APPLICATION_PROTOCOL_DEFINITION ( 'draft international standard', 'automotive_design', 1998, #12687 ) ;
#14595 = AXIS2_PLACEMENT_3D ( 'NONE', #13289, #7531, #14693 ) ;
#14596 = AXIS2_PLACEMENT_3D ( 'NONE', #7139, #7245, #21253 ) ;
#14598 = ORIENTED_EDGE ( 'NONE', *, *, #21927, .F. ) ;
#14597 = ORIENTED_EDGE ( 'NONE', *, *, #19737, .T. ) ;
#14599 = ORIENTED_EDGE ( 'NONE', *, *, #19999, .F. ) ;
#14601 = ORIENTED_EDGE ( 'NONE', *, *, #12844, .F. ) ;
#14600 = ORIENTED_EDGE ( 'NONE', *, *, #8723, .F. ) ;
#14602 = CARTESIAN_POINT ( 'NONE',  ( -89.70000000000055707, -2.700000000000084110, -1.999999999999946265 ) ) ;
#14603 = CARTESIAN_POINT ( 'NONE',  ( 8.181569977154572015, -11.86479625201664412, 7.340676138759426372 ) ) ;
#14604 = CARTESIAN_POINT ( 'NONE',  ( 2.775557561562891351E-14, 10.49999999999998579, -2.133974596215532316 ) ) ;
#14605 = DIRECTION ( 'NONE',  ( 0.000000000000000000, 1.000000000000000000, 0.000000000000000000 ) ) ;
#14606 = DIRECTION ( 'NONE',  ( 3.885780586188016830E-16, 4.437342591868156373E-31, -1.000000000000000000 ) ) ;
#14607 = CARTESIAN_POINT ( 'NONE',  ( 0.8678420939694135861, -0.5999999999999889866, 4.443813723662904280 ) ) ;
#14608 = CIRCLE ( 'NONE', #21756, 2.550000000000010481 ) ;
#14609 = CYLINDRICAL_SURFACE ( 'NONE', #11059, 4.499999999999988454 ) ;
#14610 = CARTESIAN_POINT ( 'NONE',  ( 3.534277608972077545, 1.672424706883760770, -3.378451613207327231 ) ) ;
#14611 = FACE_OUTER_BOUND ( 'NONE', #22765, .T. ) ;
#14612 = CIRCLE ( 'NONE', #10115, 2.500000000000009326 ) ;
#14613 = CARTESIAN_POINT ( 'NONE',  ( 30.00000000029184832, -9.961476088449217059E-10, -36.45000000000000284 ) ) ;
#14614 = DIRECTION ( 'NONE',  ( -1.000000000000000000, 0.000000000000000000, 0.000000000000000000 ) ) ;
#14615 = CARTESIAN_POINT ( 'NONE',  ( 4.175813232069142344, -2.061359961916364725, 3.570380186727395433 ) ) ;
#14616 = CARTESIAN_POINT ( 'NONE',  ( 8.079084010241066593, -2.020344040167372679, 6.665520415301748436 ) ) ;
#14617 = DIRECTION ( 'NONE',  ( -0.7071067811865441310, -0.7071067811865510144, 0.000000000000000000 ) ) ;
#14618 = DIRECTION ( 'NONE',  ( 1.550910762415566494E-16, 1.000000000000000000, -8.135128085091684243E-31 ) ) ;
#14619 = ADVANCED_FACE ( 'NONE', ( #5765 ), #3981, .T. ) ;
#14620 = ORIENTED_EDGE ( 'NONE', *, *, #14191, .T. ) ;
#14622 = EDGE_LOOP ( 'NONE', ( #1322, #16975, #19250 ) ) ;
#14621 = VERTEX_POINT ( 'NONE', #14471 ) ;
#14623 = EDGE_LOOP ( 'NONE', ( #10027, #9822, #3433, #19784 ) ) ;
#14624 = AXIS2_PLACEMENT_3D ( 'NONE', #5520, #16664, #5984 ) ;
#14625 = EDGE_LOOP ( 'NONE', ( #3798, #17304, #11661, #13408 ) ) ;
#14627 = ORIENTED_EDGE ( 'NONE', *, *, #17713, .T. ) ;
#14626 = EDGE_LOOP ( 'NONE', ( #3819, #1406, #11431, #15681 ) ) ;
#14628 = CIRCLE ( 'NONE', #11612, 0.4999999999999995559 ) ;
#14629 = EDGE_LOOP ( 'NONE', ( #8987, #8871, #10518, #4456 ) ) ;
#14630 = CARTESIAN_POINT ( 'NONE',  ( 124.5000000000017195, -4.500000000000003553, 6.500000000000123457 ) ) ;
#14631 = ORIENTED_EDGE ( 'NONE', *, *, #18861, .T. ) ;
#14632 = EDGE_LOOP ( 'NONE', ( #6275, #13845, #22582, #23211 ) ) ;
#14633 = DIRECTION ( 'NONE',  ( -3.330669073875432643E-16, -4.437342591868153746E-31, 1.000000000000000000 ) ) ;
#14634 = ADVANCED_FACE ( 'NONE', ( #9288 ), #16335, .T. ) ;
#14635 = AXIS2_PLACEMENT_3D ( 'NONE', #8587, #22952, #21186 ) ;
#14636 = CARTESIAN_POINT ( 'NONE',  ( 4.198928548860714649, -0.8158838809860312624, -3.526471437616904403 ) ) ;
#14637 = DIRECTION ( 'NONE',  ( -1.000000000000000000, 4.615739097524200579E-16, 1.134196829589820086E-15 ) ) ;
#14638 = PRODUCT_DEFINITION_FORMATION_WITH_SPECIFIED_SOURCE ( 'ANY', '', #14203, .NOT_KNOWN. ) ;
#14639 = PLANE ( 'NONE',  #12112 ) ;
#14640 = DIRECTION ( 'NONE',  ( 0.7071067811865535679, 0.7071067811865414665, 0.000000000000000000 ) ) ;
#14641 = CARTESIAN_POINT ( 'NONE',  ( 0.9337610948747044892, 1.709055945004937405, -4.750000000000024869 ) ) ;
#14642 = CARTESIAN_POINT ( 'NONE',  ( -2.756197834950217640, -3.027510591568727705, -3.223146290109647261 ) ) ;
#14643 = B_SPLINE_CURVE_WITH_KNOTS ( 'NONE', 3,
 ( #20850, #2953, #17052, #8127, #1312, #6370 ),
 .UNSPECIFIED., .F., .F.,
 ( 4, 2, 4 ),
 ( 0.004904496978749070882, 0.006291728866292733632, 0.007678960753836396383 ),
 .UNSPECIFIED. ) ;
#14644 = CARTESIAN_POINT ( 'NONE',  ( -56.91911807125113398, 0.5000000000000143219, -8.333333333333387216 ) ) ;
#14645 = CARTESIAN_POINT ( 'NONE',  ( 5.599999999999994316, -2.020725942163688504, 3.499999999999996003 ) ) ;
#14646 =( BOUNDED_SURFACE ( )  B_SPLINE_SURFACE ( 3, 2, ( 
 ( #12382, #19564, #10619 ),
 ( #17809, #23233, #7118 ),
 ( #3574, #19690, #10739 ),
 ( #1232, #8408, #15568 ),
 ( #6630, #13807, #4859 ),
 ( #12027, #19215, #10273 ) ),
 .UNSPECIFIED., .F., .F., .F. ) 
 B_SPLINE_SURFACE_WITH_KNOTS ( ( 4, 2, 4 ),
 ( 3, 3 ),
 ( 0.01651999345535504551, 0.01858032176739833966, 0.02064065007944163380 ),
 ( 0.000000000000000000, 1.000000000000000000 ),
 .UNSPECIFIED. ) 
 GEOMETRIC_REPRESENTATION_ITEM ( )  RATIONAL_B_SPLINE_SURFACE ( (
 ( 1.000000000000000000, 0.8047781103519392465, 1.000000000000000000),
 ( 1.000000000000000000, 0.8123785825606634203, 1.000000000000000000),
 ( 1.000000000000000000, 0.8190671539785229216, 1.000000000000000000),
 ( 1.000000000000000000, 0.8192352254837912406, 1.000000000000000000),
 ( 1.000000000000000000, 0.8126129677209334989, 1.000000000000000000),
 ( 1.000000000000000000, 0.8047712537969733404, 1.000000000000000000) ) ) 
 REPRESENTATION_ITEM ( '' )  SURFACE ( )  );
#14647 = CARTESIAN_POINT ( 'NONE',  ( -6.591949208711866959E-15, -9.999999999999971578, 12.50000000000003375 ) ) ;
#14648 = ORIENTED_EDGE ( 'NONE', *, *, #2784, .T. ) ;
#14649 = AXIS2_PLACEMENT_3D ( 'NONE', #18062, #4149, #21822 ) ;
#14651 = ORIENTED_EDGE ( 'NONE', *, *, #16585, .T. ) ;
#14650 = ORIENTED_EDGE ( 'NONE', *, *, #20020, .T. ) ;
#14652 =( REPRESENTATION_RELATIONSHIP ('NONE','NONE', #19450, #16457 ) REPRESENTATION_RELATIONSHIP_WITH_TRANSFORMATION ( #8113 )SHAPE_REPRESENTATION_RELATIONSHIP( ) );
#14653 = VERTEX_POINT ( 'NONE', #12582 ) ;
#14654 = VERTEX_POINT ( 'NONE', #10916 ) ;
#14655 = VERTEX_POINT ( 'NONE', #18110 ) ;
#14656 = EDGE_CURVE ( 'NONE', #13358, #18075, #10701, .T. ) ;
#14657 = DIRECTION ( 'NONE',  ( -2.168404344970994323E-16, 1.000000000000000000, -1.577721810442023611E-30 ) ) ;
#14658 = CARTESIAN_POINT ( 'NONE',  ( 4.330127018922103055, 4.999999999999838352, 7.499999999999971578 ) ) ;
#14659 = CARTESIAN_POINT ( 'NONE',  ( 4.151274195509686571, -2.039912954708744675, -3.533232880573493606 ) ) ;
#14660 = DIRECTION ( 'NONE',  ( 1.374679200952786429E-16, -1.000000000000000000, 0.000000000000000000 ) ) ;
#14661 = DIRECTION ( 'NONE',  ( 1.000000000000000000, 2.168404344971017743E-16, -1.780660105995169760E-30 ) ) ;
#14662 = CIRCLE ( 'NONE', #1161, 2.549999999999997158 ) ;
#14663 = CARTESIAN_POINT ( 'NONE',  ( 7.713464495932034204, -12.17135227947844811, 8.131426806228688520 ) ) ;
#14664 = CARTESIAN_POINT ( 'NONE',  ( 8.697224362267997222, -12.00000000000002842, 6.250000000000019540 ) ) ;
#14665 = CARTESIAN_POINT ( 'NONE',  ( -50.65685424949274562, 2.700000000000021938, -8.000000000000062172 ) ) ;
#14666 = FACE_OUTER_BOUND ( 'NONE', #1524, .T. ) ;
#14667 = DIRECTION ( 'NONE',  ( -7.860214984770699307E-18, 1.409037165336591006E-16, 1.000000000000000000 ) ) ;
#14668 = CARTESIAN_POINT ( 'NONE',  ( 66.26395429947837101, -4.000000000000003553, 6.500000000000110134 ) ) ;
#14669 = DIRECTION ( 'NONE',  ( -1.000000000000000000, 4.190823558986611203E-31, 1.733449886265891589E-32 ) ) ;
#14670 = DIRECTION ( 'NONE',  ( 9.693647360340828445E-26, 0.000000000000000000, -1.000000000000000000 ) ) ;
#14671 = CARTESIAN_POINT ( 'NONE',  ( 3.974167765203684866, 0.7238254970431058366, -3.565825589389272743 ) ) ;
#14672 = EDGE_CURVE ( 'NONE', #11002, #22096, #12930, .T. ) ;
#14673 = VECTOR ( 'NONE', #962, 1000.000000000000000 ) ;
#14674 = ORIENTED_EDGE ( 'NONE', *, *, #5530, .T. ) ;
#14675 = EDGE_CURVE ( 'NONE', #19219, #20477, #16211, .T. ) ;
#14676 = LINE ( 'NONE', #9501, #1962 ) ;
#14677 = CARTESIAN_POINT ( 'NONE',  ( -4.000000000000003553, -0.7779732554280798240, -5.566455648918319454 ) ) ;
#14678 = ORIENTED_EDGE ( 'NONE', *, *, #22824, .F. ) ;
#14679 = CARTESIAN_POINT ( 'NONE',  ( -6.000000000000088818, 1.999999999999960032, -17.72029585817558228 ) ) ;
#14680 = LINE ( 'NONE', #347, #10003 ) ;
#14681 = CARTESIAN_POINT ( 'NONE',  ( 4.050536630291690088, 2.401306687817042373, -2.976670123173763116 ) ) ;
#14682 = DIRECTION ( 'NONE',  ( 1.613696256722611405E-16, -0.000000000000000000, -1.000000000000000000 ) ) ;
#14683 = EDGE_CURVE ( 'NONE', #4498, #16351, #1985, .T. ) ;
#14684 = DIRECTION ( 'NONE',  ( -1.000000000000000000, 0.000000000000000000, 0.000000000000000000 ) ) ;
#14685 = DIRECTION ( 'NONE',  ( 3.032184104443272185E-30, 1.000000000000000000, -7.395570986447005381E-32 ) ) ;
#14686 = EDGE_CURVE ( 'NONE', #9743, #700, #21840, .T. ) ;
#14687 = LINE ( 'NONE', #12699, #6791 ) ;
#14688 = CARTESIAN_POINT ( 'NONE',  ( 7.332081355611500761, -13.77321347121581319, 7.890992604157081480 ) ) ;
#14689 = DIRECTION ( 'NONE',  ( 1.000000000000000000, 6.224605580259554159E-31, -2.887593071917436153E-31 ) ) ;
#14690 = CARTESIAN_POINT ( 'NONE',  ( 0.02993401039714140358, -3.373851915354621145, -1.156317065392238774 ) ) ;
#14691 = VECTOR ( 'NONE', #13514, 1000.000000000000000 ) ;
#14692 = CARTESIAN_POINT ( 'NONE',  ( -43.06238456605044007, 5.319238815542546739, -8.000000000000090594 ) ) ;
#14693 = DIRECTION ( 'NONE',  ( -0.8660254037844372643, -0.5000000000000024425, 0.000000000000000000 ) ) ;
#14694 = DIRECTION ( 'NONE',  ( 0.000000000000000000, 8.673617379884027583E-16, 1.000000000000000000 ) ) ;
#14695 = EDGE_CURVE ( 'NONE', #8098, #18939, #19645, .T. ) ;
#14696 = EDGE_CURVE ( 'NONE', #4926, #1834, #13578, .T. ) ;
#14697 = PRODUCT_CONTEXT ( 'NONE', #3962, 'mechanical' ) ;
#14698 = ORIENTED_EDGE ( 'NONE', *, *, #8247, .F. ) ;
#14700 = ORIENTED_EDGE ( 'NONE', *, *, #2092, .F. ) ;
#14699 = VERTEX_POINT ( 'NONE', #356 ) ;
#14701 = VECTOR ( 'NONE', #13141, 1000.000000000000000 ) ;
#14702 = AXIS2_PLACEMENT_3D ( 'NONE', #21868, #14023, #5088 ) ;
#14703 = EDGE_CURVE ( 'NONE', #23120, #20563, #8278, .T. ) ;
#14704 = CARTESIAN_POINT ( 'NONE',  ( 2.775557561562891351E-14, 0.5000000000000108802, -9.999999999999968026 ) ) ;
#14705 = FACE_OUTER_BOUND ( 'NONE', #16487, .T. ) ;
#14706 = CARTESIAN_POINT ( 'NONE',  ( 8.129778652391312477, -12.42126101213639444, 7.405931224841370231 ) ) ;
#14708 = ORIENTED_EDGE ( 'NONE', *, *, #10902, .T. ) ;
#14707 = EDGE_CURVE ( 'NONE', #1571, #15390, #6811, .T. ) ;
#14709 = CARTESIAN_POINT ( 'NONE',  ( 35.50000000029184832, 16.99999999900385461, -18.50000000000000355 ) ) ;
#14710 = DIRECTION ( 'NONE',  ( -1.454462294001240516E-30, -1.000000000000000000, -0.000000000000000000 ) ) ;
#14711 = EDGE_CURVE ( 'NONE', #180, #15946, #12441, .T. ) ;
#14712 = LINE ( 'NONE', #7666, #14009 ) ;
#14713 = CARTESIAN_POINT ( 'NONE',  ( 0.1425507193225079572, -0.5999999999999897637, -3.725915899842239476 ) ) ;
#14714 = DIRECTION ( 'NONE',  ( 3.032184104443272185E-30, 1.000000000000000000, -7.395570986447005381E-32 ) ) ;
#14715 = PLANE ( 'NONE',  #16632 ) ;
#14716 = EDGE_CURVE ( 'NONE', #6633, #195, #13169, .T. ) ;
#14717 = DIRECTION ( 'NONE',  ( 1.066786462891689527E-26, 6.656013887802287108E-31, 1.000000000000000000 ) ) ;
#14718 = CARTESIAN_POINT ( 'NONE',  ( -12.85000000000002807, -12.00000000000002842, 6.250000000000019540 ) ) ;
#14719 = SURFACE_STYLE_USAGE ( .BOTH. , #22375 ) ;
#14720 = DIRECTION ( 'NONE',  ( 1.066786462891689527E-26, 6.656013887802287108E-31, 1.000000000000000000 ) ) ;
#14721 = CARTESIAN_POINT ( 'NONE',  ( -6.000000000000143885, 1.999999999999960032, 8.000000000000062172 ) ) ;
#14722 = DIRECTION ( 'NONE',  ( -0.000000000000000000, -0.000000000000000000, 1.000000000000000000 ) ) ;
#14723 = VECTOR ( 'NONE', #10949, 1000.000000000000000 ) ;
#14724 = CIRCLE ( 'NONE', #2697, 4.000000000000045297 ) ;
#14725 = CARTESIAN_POINT ( 'NONE',  ( 0.1388410611046089760, 2.351840044243042716, -2.926493552096025130 ) ) ;
#14726 = CARTESIAN_POINT ( 'NONE',  ( 8.148407558030074327, -0.5601289046717625730, 7.382406087063999145 ) ) ;
#14727 = AXIS2_PLACEMENT_3D ( 'NONE', #13746, #20928, #4794 ) ;
#14728 = ORIENTED_EDGE ( 'NONE', *, *, #15233, .T. ) ;
#14729 = FILL_AREA_STYLE_COLOUR ( '', #6744 ) ;
#14731 = ORIENTED_EDGE ( 'NONE', *, *, #4503, .T. ) ;
#14730 = EDGE_LOOP ( 'NONE', ( #33, #13501, #2411, #12982 ) ) ;
#14732 = VERTEX_POINT ( 'NONE', #4446 ) ;
#14733 = ORIENTED_EDGE ( 'NONE', *, *, #15426, .F. ) ;
#14735 = ORIENTED_EDGE ( 'NONE', *, *, #15566, .F. ) ;
#14734 = ORIENTED_EDGE ( 'NONE', *, *, #594, .F. ) ;
#14736 = AXIS2_PLACEMENT_3D ( 'NONE', #13915, #19330, #17317 ) ;
#14737 = ORIENTED_EDGE ( 'NONE', *, *, #20882, .T. ) ;
#14738 = ADVANCED_FACE ( 'NONE', ( #22345 ), #22222, .T. ) ;
#14739 = DIRECTION ( 'NONE',  ( -0.6819983600625060260, -0.7313537016191635765, -6.106365041599011361E-16 ) ) ;
#14740 = EDGE_LOOP ( 'NONE', ( #402, #18732, #11236, #9764 ) ) ;
#14741 = ORIENTED_EDGE ( 'NONE', *, *, #15183, .T. ) ;
#14742 = CARTESIAN_POINT ( 'NONE',  ( 0.5732283800867107315, 0.6000000000000134115, 4.263122468548279365 ) ) ;
#14743 = CIRCLE ( 'NONE', #15853, 0.4999999999999995559 ) ;
#14744 = CARTESIAN_POINT ( 'NONE',  ( 4.204015924366130363, -1.626724848190950867, -3.610627190413379317 ) ) ;
#14745 = DIRECTION ( 'NONE',  ( -0.7313537016191756779, 0.6819983600624930364, -4.478224685260177339E-16 ) ) ;
#14746 = CIRCLE ( 'NONE', #7615, 2.099999999999999645 ) ;
#14747 = EDGE_CURVE ( 'NONE', #21589, #20222, #13284, .T. ) ;
#14748 = LINE ( 'NONE', #16613, #18506 ) ;
#14749 = CIRCLE ( 'NONE', #856, 2.550000000000000711 ) ;
#14750 = CARTESIAN_POINT ( 'NONE',  ( 2.775557561562891351E-14, 7.999999999999983125, -0.4999999999999865663 ) ) ;
#14751 = DIRECTION ( 'NONE',  ( 1.436408664093593395E-16, -0.5454545454545469685, 0.8381404052084432399 ) ) ;
#14752 = DIRECTION ( 'NONE',  ( -1.000000000000000000, -0.000000000000000000, 0.000000000000000000 ) ) ;
#14753 = APPLICATION_CONTEXT ( 'automotive_design' ) ;
#14754 = FACE_OUTER_BOUND ( 'NONE', #14988, .T. ) ;
#14755 = CARTESIAN_POINT ( 'NONE',  ( 0.2182387239031300108, 1.693823289467299098, -3.500000000000034639 ) ) ;
#14756 = DIRECTION ( 'NONE',  ( 1.454462294001240516E-30, 1.000000000000000000, 0.000000000000000000 ) ) ;
#14757 = ORIENTED_EDGE ( 'NONE', *, *, #18050, .F. ) ;
#14758 = UNCERTAINTY_MEASURE_WITH_UNIT (LENGTH_MEASURE( 1.000000000000000082E-05 ), #9214, 'distance_accuracy_value', 'NONE');
#14759 = TOROIDAL_SURFACE ( 'NONE', #7625, 2.250000000000000444, 0.2500000000000000000 ) ;
#14760 =( LENGTH_UNIT ( ) NAMED_UNIT ( * ) SI_UNIT ( .MILLI., .METRE. ) );
#14761 = CARTESIAN_POINT ( 'NONE',  ( -3.092826256371965993E-14, 60.00000000000000000, 4.249999999999983125 ) ) ;
#14762 = AXIS2_PLACEMENT_3D ( 'NONE', #990, #15661, #6511 ) ;
#14763 = B_SPLINE_CURVE_WITH_KNOTS ( 'NONE', 3,
 ( #15430, #17540, #17192, #6501, #12129, #11664 ),
 .UNSPECIFIED., .F., .F.,
 ( 4, 2, 4 ),
 ( 0.000000000000000000, 0.002086519881787258883, 0.004173039763574517766 ),
 .UNSPECIFIED. ) ;
#14765 = ORIENTED_EDGE ( 'NONE', *, *, #12022, .F. ) ;
#14764 = EDGE_LOOP ( 'NONE', ( #12417, #22330, #20623, #11923 ) ) ;
#14766 = CIRCLE ( 'NONE', #8390, 0.4999999999999990563 ) ;
#14767 = VECTOR ( 'NONE', #14520, 1000.000000000000114 ) ;
#14768 = CONICAL_SURFACE ( 'NONE', #16267, 2.054999999999999716, 0.7853981633974502774 ) ;
#14769 = EDGE_LOOP ( 'NONE', ( #4601, #14960, #6358, #2489 ) ) ;
#14770 = EDGE_LOOP ( 'NONE', ( #14018, #22822, #5380, #12569 ) ) ;
#14771 = ORIENTED_EDGE ( 'NONE', *, *, #19029, .F. ) ;
#14772 = EDGE_LOOP ( 'NONE', ( #22764, #9947 ) ) ;
#14773 = DIRECTION ( 'NONE',  ( 3.885780586188016830E-16, 4.437342591868156373E-31, -1.000000000000000000 ) ) ;
#14774 = DIRECTION ( 'NONE',  ( 7.860214984770699307E-18, -1.409037165336591006E-16, -1.000000000000000000 ) ) ;
#14775 = EDGE_CURVE ( 'NONE', #11516, #13735, #2297, .T. ) ;
#14776 = CARTESIAN_POINT ( 'NONE',  ( -6.000000000000116351, 7.499999999999958256, -7.500000000000062172 ) ) ;
#14777 = CIRCLE ( 'NONE', #4631, 2.500000000000000444 ) ;
#14778 = CARTESIAN_POINT ( 'NONE',  ( -4.330127018922255822, -9.714451465470119729E-14, 7.499999999999985789 ) ) ;
#14779 = CIRCLE ( 'NONE', #14436, 2.550000000000003819 ) ;
#14780 = FACE_OUTER_BOUND ( 'NONE', #3358, .T. ) ;
#14781 = FACE_OUTER_BOUND ( 'NONE', #16972, .T. ) ;
#14782 = AXIS2_PLACEMENT_3D ( 'NONE', #4376, #17518, #20950 ) ;
#14783 = AXIS2_PLACEMENT_3D ( 'NONE', #6622, #15665, #5094 ) ;
#14784 = FACE_BOUND ( 'NONE', #22970, .T. ) ;
#14785 = CIRCLE ( 'NONE', #158, 0.5000000000000029976 ) ;
#14786 = AXIS2_PLACEMENT_3D ( 'NONE', #16121, #12477, #377 ) ;
#14787 = CARTESIAN_POINT ( 'NONE',  ( -4.000000000000003553, 2.309401076758532678, -5.242734410091827613 ) ) ;
#14788 = CARTESIAN_POINT ( 'NONE',  ( -47.82842712474642610, -4.371572875253856516, 8.000000000000076383 ) ) ;
#14789 = CARTESIAN_POINT ( 'NONE',  ( 0.000000000000000000, 0.000000000000000000, 0.000000000000000000 ) ) ;
#14790 = CARTESIAN_POINT ( 'NONE',  ( -4.229990831856726530, 1.750000000000057732, -2.173440963673431536 ) ) ;
#14791 = EDGE_CURVE ( 'NONE', #11179, #12651, #14444, .T. ) ;
#14792 = CARTESIAN_POINT ( 'NONE',  ( 2.775557561562891351E-14, 0.000000000000000000, -0.4999999999999865663 ) ) ;
#14793 = CARTESIAN_POINT ( 'NONE',  ( 0.03027795056225613193, 0.6888063905605182891, 3.499999999999994671 ) ) ;
#14794 = VECTOR ( 'NONE', #12787, 1000.000000000000000 ) ;
#14795 = CIRCLE ( 'NONE', #20080, 3.500000000000013323 ) ;
#14796 = VERTEX_POINT ( 'NONE', #2453 ) ;
#14797 = AXIS2_PLACEMENT_3D ( 'NONE', #6334, #13385, #8323 ) ;
#14798 = FACE_OUTER_BOUND ( 'NONE', #21723, .T. ) ;
#14799 = CARTESIAN_POINT ( 'NONE',  ( 57.15235153779114796, -1.074585193523325266, 6.000000000000185629 ) ) ;
#14800 = ORIENTED_EDGE ( 'NONE', *, *, #9519, .T. ) ;
#14801 = DIRECTION ( 'NONE',  ( -0.7313537016191745677, -0.6819983600624940356, -1.072890437865584285E-16 ) ) ;
#14802 = CARTESIAN_POINT ( 'NONE',  ( -4.000000000000003553, -2.309401076758532678, -5.242734410091827613 ) ) ;
#14803 = CARTESIAN_POINT ( 'NONE',  ( 108.2426266706970637, -6.527605602963671316, -5.999999999999991118 ) ) ;
#14804 = DIRECTION ( 'NONE',  ( -7.860214984770699307E-18, 1.409037165336591006E-16, 1.000000000000000000 ) ) ;
#14805 = DIRECTION ( 'NONE',  ( -1.756300210255732376E-61, 4.190823558986625216E-31, 1.000000000000000000 ) ) ;
#14806 = DIRECTION ( 'NONE',  ( 5.551115123125796261E-17, -2.869019762633797485E-16, -1.000000000000000000 ) ) ;
#14807 = DIRECTION ( 'NONE',  ( -2.168404344970994323E-16, 1.000000000000000000, -1.577721810442023611E-30 ) ) ;
#14808 = LINE ( 'NONE', #11387, #3874 ) ;
#14809 = DIRECTION ( 'NONE',  ( -2.220446049250313081E-16, 1.000000000000000000, -7.025792437124636392E-31 ) ) ;
#14810 = AXIS2_PLACEMENT_3D ( 'NONE', #19205, #20981, #4618 ) ;
#14811 = CARTESIAN_POINT ( 'NONE',  ( 29.00000000029184832, 16.99999999900385461, -26.00000000000000000 ) ) ;
#14812 = B_SPLINE_CURVE_WITH_KNOTS ( 'NONE', 3,
 ( #19861, #8926, #21524, #19625, #21285, #7392 ),
 .UNSPECIFIED., .F., .F.,
 ( 4, 2, 4 ),
 ( 0.000000000000000000, 0.002086519881787257148, 0.004173039763574514296 ),
 .UNSPECIFIED. ) ;
#14813 = AXIS2_PLACEMENT_3D ( 'NONE', #22374, #10132, #8361 ) ;
#14814 = DIRECTION ( 'NONE',  ( -1.000000000000000000, 4.190823558986610327E-31, -1.733449886265890494E-32 ) ) ;
#14815 = DIRECTION ( 'NONE',  ( 0.6819983600624998088, -0.7313537016191693496, 0.000000000000000000 ) ) ;
#14816 = B_SPLINE_CURVE_WITH_KNOTS ( 'NONE', 3,
 ( #9263, #7280, #18548, #12665, #16312, #5738, #22081, #3958, #16528, #12910, #215, #2427, #19966, #21739 ),
 .UNSPECIFIED., .F., .F.,
 ( 4, 2, 2, 2, 2, 2, 4 ),
 ( 0.000000000000000000, 0.0008860460682957648024, 0.001772092136591529605, 0.002215115170739412331, 0.002658138204887295492, 0.003101161239035177784, 0.003544184273183060944 ),
 .UNSPECIFIED. ) ;
#14817 = AXIS2_PLACEMENT_3D ( 'NONE', #21621, #12655, #9138 ) ;
#14818 = EDGE_CURVE ( 'NONE', #9975, #11731, #5315, .T. ) ;
#14819 = FACE_BOUND ( 'NONE', #18764, .T. ) ;
#14820 = AXIS2_PLACEMENT_3D ( 'NONE', #15208, #18863, #414 ) ;
#14821 = EDGE_CURVE ( 'NONE', #22298, #15772, #11681, .T. ) ;
#14822 = ITEM_DEFINED_TRANSFORMATION ( 'NONE', 'NONE', #17261,  #22115 ) ;
#14823 = B_SPLINE_CURVE_WITH_KNOTS ( 'NONE', 3,
 ( #6021, #612, #21902, #6135, #4230, #9658 ),
 .UNSPECIFIED., .F., .F.,
 ( 4, 2, 4 ),
 ( 0.002336974151641528670, 0.003500975885716446721, 0.004664977619791364771 ),
 .UNSPECIFIED. ) ;
#14824 = VERTEX_POINT ( 'NONE', #1054 ) ;
#14825 = EDGE_CURVE ( 'NONE', #5698, #13412, #7983, .T. ) ;
#14826 = VECTOR ( 'NONE', #14241, 1000.000000000000000 ) ;
#14828 = ORIENTED_EDGE ( 'NONE', *, *, #1810, .T. ) ;
#14827 = VERTEX_POINT ( 'NONE', #816 ) ;
#14829 = CARTESIAN_POINT ( 'NONE',  ( 2.775557561562891351E-14, 2.499999999999995115, -12.99999999999999822 ) ) ;
#14830 = DIRECTION ( 'NONE',  ( 1.000000000000000000, 1.479114197289397135E-31, 5.916456789157588541E-31 ) ) ;
#14831 = LINE ( 'NONE', #5895, #9015 ) ;
#14832 = ORIENTED_EDGE ( 'NONE', *, *, #4937, .T. ) ;
#14833 = DIRECTION ( 'NONE',  ( 1.000000000000000000, -2.168404344971005170E-16, 1.203141491611682442E-30 ) ) ;
#14834 = DIRECTION ( 'NONE',  ( 1.066786462891689527E-26, 6.656013887802287108E-31, 1.000000000000000000 ) ) ;
#14835 = CARTESIAN_POINT ( 'NONE',  ( 1.318516776095790322, 3.857556137907070859, -5.600000000000003197 ) ) ;
#14837 = ADVANCED_FACE ( 'NONE', ( #6227 ), #18575, .T. ) ;
#14836 = LINE ( 'NONE', #11189, #19421 ) ;
#14838 = ADVANCED_FACE ( 'NONE', ( #16783 ), #11275, .T. ) ;
#14839 = PLANE ( 'NONE',  #8048 ) ;
#14840 = LINE ( 'NONE', #21798, #13969 ) ;
#14841 = DIRECTION ( 'NONE',  ( 4.190823558986625216E-31, -1.000000000000000000, 4.190823558986625216E-31 ) ) ;
#14842 =( LENGTH_UNIT ( ) NAMED_UNIT ( * ) SI_UNIT ( .MILLI., .METRE. ) );
#14843 = CARTESIAN_POINT ( 'NONE',  ( 24.99999999999995737, 2.000000000000001776, -17.49999999999998224 ) ) ;
#14844 = ADVANCED_FACE ( 'NONE', ( #7749 ), #5878, .F. ) ;
#14845 = CARTESIAN_POINT ( 'NONE',  ( 1.321505333908973290, -3.855830693249184815, -5.565789719053443996 ) ) ;
#14846 = VECTOR ( 'NONE', #10326, 1000.000000000000000 ) ;
#14847 = DIRECTION ( 'NONE',  ( -1.000000000000000000, 0.000000000000000000, 0.000000000000000000 ) ) ;
#14848 = CARTESIAN_POINT ( 'NONE',  ( 3.999999999999937828, -0.3979232138631629834, 4.499947235583196612E-14 ) ) ;
#14849 = CARTESIAN_POINT ( 'NONE',  ( 7.490313984279763915, -0.1442844712671001728, 7.566633644154783234 ) ) ;
#14850 = ORIENTED_EDGE ( 'NONE', *, *, #11456, .T. ) ;
#14851 = EDGE_CURVE ( 'NONE', #12208, #4062, #22106, .T. ) ;
#14852 =( LENGTH_UNIT ( ) NAMED_UNIT ( * ) SI_UNIT ( .MILLI., .METRE. ) );
#14854 = ORIENTED_EDGE ( 'NONE', *, *, #474, .T. ) ;
#14853 = ORIENTED_EDGE ( 'NONE', *, *, #7340, .F. ) ;
#14855 = ORIENTED_EDGE ( 'NONE', *, *, #6455, .F. ) ;
#14857 = EDGE_LOOP ( 'NONE', ( #1972, #17533, #7995, #13821 ) ) ;
#14856 = ORIENTED_EDGE ( 'NONE', *, *, #4653, .T. ) ;
#14858 = ORIENTED_EDGE ( 'NONE', *, *, #2062, .T. ) ;
#14859 = CARTESIAN_POINT ( 'NONE',  ( -4.113620667976075396, -1.750000000000001554, 2.374999999999986677 ) ) ;
#14860 = ORIENTED_EDGE ( 'NONE', *, *, #20127, .F. ) ;
#14861 = ORIENTED_EDGE ( 'NONE', *, *, #6967, .F. ) ;
#14862 = DIRECTION ( 'NONE',  ( 0.000000000000000000, 0.000000000000000000, 1.000000000000000000 ) ) ;
#14863 = DIRECTION ( 'NONE',  ( -0.000000000000000000, -0.000000000000000000, 1.000000000000000000 ) ) ;
#14864 =( LENGTH_UNIT ( ) NAMED_UNIT ( * ) SI_UNIT ( .MILLI., .METRE. ) );
#14865 = ADVANCED_FACE ( 'NONE', ( #20696 ), #19585, .T. ) ;
#14866 = CARTESIAN_POINT ( 'NONE',  ( 124.5000000000019469, -7.000000000000062172, 2.081668171172168513E-14 ) ) ;
#14867 = EDGE_CURVE ( 'NONE', #7024, #7626, #5691, .T. ) ;
#14868 = PLANE ( 'NONE',  #18122 ) ;
#14869 = EDGE_CURVE ( 'NONE', #6492, #6466, #9444, .T. ) ;
#14870 = DIRECTION ( 'NONE',  ( 1.000000000000000000, -4.190823558986610327E-31, 1.733449886265890494E-32 ) ) ;
#14871 = DIRECTION ( 'NONE',  ( -0.7313537016191767881, -0.6819983600624918152, -4.403559511741033569E-16 ) ) ;
#14872 = LINE ( 'NONE', #20292, #19694 ) ;
#14873 = FILL_AREA_STYLE_COLOUR ( '', #15094 ) ;
#14874 = B_SPLINE_CURVE_WITH_KNOTS ( 'NONE', 3,
 ( #19059, #13882, #4709, #10226 ),
 .UNSPECIFIED., .F., .F.,
 ( 4, 4 ),
 ( 2.380735702043793293E-07, 0.002775112046896986880 ),
 .UNSPECIFIED. ) ;
#14875 = PRESENTATION_LAYER_ASSIGNMENT (  '', '', ( #12233 ) ) ;
#14876 = DIRECTION ( 'NONE',  ( 1.333893503340766797E-15, -2.778352770574087576E-17, -1.000000000000000000 ) ) ;
#14877 = EDGE_CURVE ( 'NONE', #3943, #7856, #1926, .T. ) ;
#14878 = CARTESIAN_POINT ( 'NONE',  ( 37.73505106183078794, 10.99999999999229239, -2.264948938166786441 ) ) ;
#14879 = ORIENTED_EDGE ( 'NONE', *, *, #14002, .T. ) ;
#14880 =( NAMED_UNIT ( * ) PLANE_ANGLE_UNIT ( ) SI_UNIT ( $, .RADIAN. ) );
#14881 = DIRECTION ( 'NONE',  ( -1.333893503340774882E-15, -2.778352770573747380E-17, -1.000000000000000000 ) ) ;
#14883 = ORIENTED_EDGE ( 'NONE', *, *, #44, .F. ) ;
#14882 = ORIENTED_EDGE ( 'NONE', *, *, #19209, .T. ) ;
#14884 = EDGE_LOOP ( 'NONE', ( #11460, #2821, #6871, #18074 ) ) ;
#14885 = ORIENTED_EDGE ( 'NONE', *, *, #6698, .F. ) ;
#14886 = COLOUR_RGB ( '', 0.72549020, 0.75294118, 0.79215686) ;
#14887 = EDGE_LOOP ( 'NONE', ( #4225, #10776, #16658, #16394, #1884, #4027, #2441, #1239, #6011, #18300, #3765, #3736 ) ) ;
#14888 = DIRECTION ( 'NONE',  ( 1.000000000000000000, 0.000000000000000000, 0.000000000000000000 ) ) ;
#14889 = CARTESIAN_POINT ( 'NONE',  ( 4.000000000000003553, 2.309401076758525573, -0.3572655899081733644 ) ) ;
#14890 = VERTEX_POINT ( 'NONE', #13964 ) ;
#14891 = CARTESIAN_POINT ( 'NONE',  ( 5.600000000000000533, -4.041451884327432076, -6.938893903907228378E-15 ) ) ;
#14892 = CARTESIAN_POINT ( 'NONE',  ( 6.000000000291855429, -9.961476088449217059E-10, -41.55000000000000426 ) ) ;
#14893 = CARTESIAN_POINT ( 'NONE',  ( 0.000000000000000000, 0.000000000000000000, 0.000000000000000000 ) ) ;
#14894 = CARTESIAN_POINT ( 'NONE',  ( -91.02295700146262902, 0.5000000000000073275, 6.338518968055040226 ) ) ;
#14895 = CARTESIAN_POINT ( 'NONE',  ( -8.723547172042716014, -11.98401194435532879, 6.817515300136823164 ) ) ;
#14896 = LINE ( 'NONE', #14665, #4915 ) ;
#14897 = FACE_OUTER_BOUND ( 'NONE', #9793, .T. ) ;
#14898 = AXIS2_PLACEMENT_3D ( 'NONE', #8040, #9801, #4375 ) ;
#14899 = DIRECTION ( 'NONE',  ( 2.013525853228507892E-32, 6.902532920683810383E-31, -1.000000000000000000 ) ) ;
#14900 = EDGE_CURVE ( 'NONE', #6614, #3480, #18458, .T. ) ;
#14901 = LINE ( 'NONE', #14553, #13756 ) ;
#14902 = TOROIDAL_SURFACE ( 'NONE', #7751, 3.500000000000000000, 0.5000000000000000000 ) ;
#14903 = DIRECTION ( 'NONE',  ( 1.298062744027682297E-32, -6.902532920683810383E-31, 1.000000000000000000 ) ) ;
#14904 = DIRECTION ( 'NONE',  ( 0.3420201433256619405, 2.669666112250838244E-16, 0.9396926207859108704 ) ) ;
#14905 = ORIENTED_EDGE ( 'NONE', *, *, #19882, .F. ) ;
#14906 = ADVANCED_FACE ( 'NONE', ( #12193 ), #1189, .T. ) ;
#14907 = EDGE_LOOP ( 'NONE', ( #19055, #21591, #14850, #19051 ) ) ;
#14908 = DIRECTION ( 'NONE',  ( -0.1556420233463033653, 0.000000000000000000, -0.9878135252003128475 ) ) ;
#14909 = DIRECTION ( 'NONE',  ( -1.733449886265891589E-32, 4.190823558986610327E-31, -1.000000000000000000 ) ) ;
#14910 =( BOUNDED_SURFACE ( )  B_SPLINE_SURFACE ( 3, 2, ( 
 ( #13959, #23158, #10320 ),
 ( #17489, #7038, #15725 ),
 ( #14209, #21398, #15831 ),
 ( #5268, #13529, #5388 ),
 ( #14317, #12428, #19610 ),
 ( #7157, #8153, #12657 ) ),
 .UNSPECIFIED., .F., .F., .F. ) 
 B_SPLINE_SURFACE_WITH_KNOTS ( ( 4, 2, 4 ),
 ( 3, 3 ),
 ( 0.01651999345535504551, 0.01858032176739834312, 0.02064065007944163727 ),
 ( 0.000000000000000000, 1.000000000000000000 ),
 .UNSPECIFIED. ) 
 GEOMETRIC_REPRESENTATION_ITEM ( )  RATIONAL_B_SPLINE_SURFACE ( (
 ( 1.000000000000000000, 0.8047781103519390244, 1.000000000000000000),
 ( 1.000000000000000000, 0.8123785825604538102, 1.000000000000000000),
 ( 1.000000000000000000, 0.8190671539788021427, 1.000000000000000000),
 ( 1.000000000000000000, 0.8192352254835137959, 1.000000000000000000),
 ( 1.000000000000000000, 0.8126129677211418878, 1.000000000000000000),
 ( 1.000000000000000000, 0.8047712537969714530, 1.000000000000000000) ) ) 
 REPRESENTATION_ITEM ( '' )  SURFACE ( )  );
#14911 = EDGE_LOOP ( 'NONE', ( #22963, #3054, #10716, #14281 ) ) ;
#14912 = CARTESIAN_POINT ( 'NONE',  ( -1.387778780781445676E-14, 2.000000000000001776, -2.000000000000001776 ) ) ;
#14913 = CARTESIAN_POINT ( 'NONE',  ( -0.6543461111163909605, -4.241015250120827140, -5.460849780464843484 ) ) ;
#14914 = CIRCLE ( 'NONE', #23202, 5.749999999999992006 ) ;
#14915 = CARTESIAN_POINT ( 'NONE',  ( -1.387778780781445676E-14, 0.2500000000000140998, 0.000000000000000000 ) ) ;
#14916 = DIRECTION ( 'NONE',  ( 1.858632295689435609E-16, 1.000000000000000000, 0.000000000000000000 ) ) ;
#14917 = VECTOR ( 'NONE', #6965, 1000.000000000000000 ) ;
#14918 = CARTESIAN_POINT ( 'NONE',  ( 5.600000000000000533, 2.020725942163695166, -3.500000000000034195 ) ) ;
#14919 = DIRECTION ( 'NONE',  ( -2.220446049250313081E-16, 1.000000000000000000, -7.025792437124636392E-31 ) ) ;
#14920 = AXIS2_PLACEMENT_3D ( 'NONE', #20363, #20258, #2251 ) ;
#14921 = DIRECTION ( 'NONE',  ( 1.000000000000000000, 1.424116703980846297E-16, -1.095779650622964657E-32 ) ) ;
#14922 = CARTESIAN_POINT ( 'NONE',  ( 5.100000000000004974, -6.249257483547704998E-31, 5.200000000000001066 ) ) ;
#14923 = CARTESIAN_POINT ( 'NONE',  ( 7.920269128372694922, -13.36773923605932346, 7.713069291591548193 ) ) ;
#14924 = TOROIDAL_SURFACE ( 'NONE', #15285, 3.113037248396092416, 1.500000000000000000 ) ;
#14925 = CARTESIAN_POINT ( 'NONE',  ( -8.954763739086851970, -1.500000000000001332, 6.678571428571422608 ) ) ;
#14926 = DIRECTION ( 'NONE',  ( -1.066605682267575422E-26, 0.000000000000000000, -1.000000000000000000 ) ) ;
#14927 = B_SPLINE_CURVE_WITH_KNOTS ( 'NONE', 3,
 ( #15464, #4994, #15693, #8646 ),
 .UNSPECIFIED., .F., .F.,
 ( 4, 4 ),
 ( 0.002080789711329279756, 0.004173039763574516031 ),
 .UNSPECIFIED. ) ;
#14928 = CARTESIAN_POINT ( 'NONE',  ( -6.999999999708142795, 35.99999999900384751, -22.50000000000000000 ) ) ;
#14929 = AXIS2_PLACEMENT_3D ( 'NONE', #15209, #2747, #15442 ) ;
#14930 = DIRECTION ( 'NONE',  ( 5.551115123125782702E-16, 1.201780285297635172E-31, -1.000000000000000000 ) ) ;
#14931 = VECTOR ( 'NONE', #2, 1000.000000000000000 ) ;
#14932 = ITEM_DEFINED_TRANSFORMATION ( 'NONE', 'NONE', #9765,  #22115 ) ;
#14933 = VERTEX_POINT ( 'NONE', #23041 ) ;
#14934 = VECTOR ( 'NONE', #18109, 1000.000000000000000 ) ;
#14935 = AXIS2_PLACEMENT_3D ( 'NONE', #20145, #11652, #14847 ) ;
#14937 = ORIENTED_EDGE ( 'NONE', *, *, #14711, .T. ) ;
#14936 = ORIENTED_EDGE ( 'NONE', *, *, #456, .T. ) ;
#14938 = CARTESIAN_POINT ( 'NONE',  ( 0.000000000000000000, 0.000000000000000000, 0.000000000000000000 ) ) ;
#14939 = VECTOR ( 'NONE', #4047, 1000.000000000000000 ) ;
#14940 = DIRECTION ( 'NONE',  ( 4.190823558986625216E-31, -1.000000000000000000, 4.190823558986625216E-31 ) ) ;
#14941 = ADVANCED_FACE ( 'NONE', ( #15732 ), #5211, .T. ) ;
#14942 = SURFACE_SIDE_STYLE ('',( #7767 ) ) ;
#14943 = DIRECTION ( 'NONE',  ( 0.000000000000000000, 0.000000000000000000, 1.000000000000000000 ) ) ;
#14944 = DIRECTION ( 'NONE',  ( 0.000000000000000000, 0.000000000000000000, 1.000000000000000000 ) ) ;
#14945 = CARTESIAN_POINT ( 'NONE',  ( -4.000000000000003553, -2.309401076758525573, -5.600000000000000533 ) ) ;
#14946 = VECTOR ( 'NONE', #15211, 1000.000000000000000 ) ;
#14947 = CARTESIAN_POINT ( 'NONE',  ( 0.2271987153435755802, -0.5999999999999894307, 3.878866322980159431 ) ) ;
#14948 = CARTESIAN_POINT ( 'NONE',  ( 0.000000000000000000, 4.041451884327362798, -2.081668171172168513E-14 ) ) ;
#14949 = DIRECTION ( 'NONE',  ( -3.885780586188016830E-16, -4.437342591868156373E-31, 1.000000000000000000 ) ) ;
#14950 = CARTESIAN_POINT ( 'NONE',  ( -4.330127018922248716, 4.689110867544532546, 7.500000000000007105 ) ) ;
#14951 = FILL_AREA_STYLE_COLOUR ( '', #9121 ) ;
#14952 = DIRECTION ( 'NONE',  ( -7.027852765209222375E-16, -0.4999999999999999445, 0.8660254037844387076 ) ) ;
#14953 = AXIS2_PLACEMENT_3D ( 'NONE', #6006, #20348, #14694 ) ;
#14954 = CARTESIAN_POINT ( 'NONE',  ( 25.60000000000000142, 6.951083313223974888E-32, 2.054999999999995719 ) ) ;
#14955 = TOROIDAL_SURFACE ( 'NONE', #4816, 6.000000000000000000, 0.5000000000000000000 ) ;
#14956 = CARTESIAN_POINT ( 'NONE',  ( 42.00000000000012079, 8.000000000000003553, -12.49999999999999645 ) ) ;
#14957 = DIRECTION ( 'NONE',  ( -9.121204216617949000E-31, -1.000000000000000000, 6.982962677686261977E-15 ) ) ;
#14958 = CARTESIAN_POINT ( 'NONE',  ( -10.49999999999999467, -13.50000000000000888, 9.250000000000035527 ) ) ;
#14959 = ORIENTED_EDGE ( 'NONE', *, *, #22338, .F. ) ;
#14961 = ORIENTED_EDGE ( 'NONE', *, *, #2313, .F. ) ;
#14960 = ORIENTED_EDGE ( 'NONE', *, *, #10946, .F. ) ;
#14962 = AXIS2_PLACEMENT_3D ( 'NONE', #15185, #16824, #4720 ) ;
#14963 = VERTEX_POINT ( 'NONE', #13860 ) ;
#14964 = ADVANCED_FACE ( 'NONE', ( #10557 ), #17728, .F. ) ;
#14965 = ORIENTED_EDGE ( 'NONE', *, *, #13147, .T. ) ;
#14967 = ORIENTED_EDGE ( 'NONE', *, *, #8224, .T. ) ;
#14966 = EDGE_LOOP ( 'NONE', ( #1602, #2872, #1544, #22946 ) ) ;
#14968 = EDGE_LOOP ( 'NONE', ( #2969, #311, #17684, #13499 ) ) ;
#14969 = DIRECTION ( 'NONE',  ( -0.7313537016191755669, 0.6819983600624931475, -2.390712761620034777E-15 ) ) ;
#14970 = ORIENTED_EDGE ( 'NONE', *, *, #3919, .F. ) ;
#14971 = EDGE_CURVE ( 'NONE', #21501, #14225, #21104, .T. ) ;
#14972 = EDGE_LOOP ( 'NONE', ( #6151, #21364, #1205, #16060 ) ) ;
#14973 = CYLINDRICAL_SURFACE ( 'NONE', #15569, 0.5000000000000038858 ) ;
#14974 = AXIS2_PLACEMENT_3D ( 'NONE', #17987, #8811, #9158 ) ;
#14975 = CARTESIAN_POINT ( 'NONE',  ( 0.3126073911695753660, -2.020725942163792421, -3.499999999999996891 ) ) ;
#14976 = CARTESIAN_POINT ( 'NONE',  ( -3.999999999708139686, 49.99999999900385461, -15.99999999999999289 ) ) ;
#14977 = CYLINDRICAL_SURFACE ( 'NONE', #22924, 0.5000000000000038858 ) ;
#14978 = CARTESIAN_POINT ( 'NONE',  ( -7.802869476033446716, -2.356467536663312767, 7.917139222842923374 ) ) ;
#14979 = EDGE_CURVE ( 'NONE', #20968, #2644, #3724, .T. ) ;
#14980 = DIRECTION ( 'NONE',  ( -1.066786462891689527E-26, -6.656013887802287108E-31, -1.000000000000000000 ) ) ;
#14981 = DIRECTION ( 'NONE',  ( -2.172745813409349776E-17, 1.000000000000000000, -1.309377075419428048E-16 ) ) ;
#14982 = ADVANCED_FACE ( 'NONE', ( #7274 ), #16926, .T. ) ;
#14983 = DIRECTION ( 'NONE',  ( 1.000000000000000000, 0.000000000000000000, 0.000000000000000000 ) ) ;
#14984 = SURFACE_SIDE_STYLE ('',( #9586 ) ) ;
#14985 =( GEOMETRIC_REPRESENTATION_CONTEXT ( 3 ) GLOBAL_UNCERTAINTY_ASSIGNED_CONTEXT ( ( #884 ) ) GLOBAL_UNIT_ASSIGNED_CONTEXT ( ( #16510, #11458, #20181 ) ) REPRESENTATION_CONTEXT ( 'NONE', 'WORKASPACE' ) );
#14986 = CARTESIAN_POINT ( 'NONE',  ( 0.000000000000000000, 0.000000000000000000, -0.3080913168122707546 ) ) ;
#14987 = CARTESIAN_POINT ( 'NONE',  ( 4.158921444904713383, -2.089933220600047825, -3.500000000000007105 ) ) ;
#14988 = EDGE_LOOP ( 'NONE', ( #19027, #20785, #11486, #8424, #1463, #16139 ) ) ;
#14989 = PRODUCT_DEFINITION_CONTEXT ( 'detailed design', #9083, 'design' ) ;
#14990 = AXIS2_PLACEMENT_3D ( 'NONE', #10768, #1829, #9013 ) ;
#14992 = ORIENTED_EDGE ( 'NONE', *, *, #10990, .T. ) ;
#14991 = VERTEX_POINT ( 'NONE', #21514 ) ;
#14993 = EDGE_CURVE ( 'NONE', #15165, #7024, #7563, .T. ) ;
#14994 = EDGE_LOOP ( 'NONE', ( #2787, #15304, #5919, #1156 ) ) ;
#14995 = ADVANCED_FACE ( 'NONE', ( #323 ), #2670, .T. ) ;
#14996 = EDGE_CURVE ( 'NONE', #7710, #8077, #10920, .T. ) ;
#14997 = ORIENTED_EDGE ( 'NONE', *, *, #14996, .F. ) ;
#14998 = ORIENTED_EDGE ( 'NONE', *, *, #18013, .T. ) ;
#14999 = DIRECTION ( 'NONE',  ( 0.000000000000000000, -1.000000000000000000, 0.000000000000000000 ) ) ;
#15000 = DIRECTION ( 'NONE',  ( 0.4999999999999997780, 5.044886816051349048E-16, 0.8660254037844387076 ) ) ;
#15001 = EDGE_CURVE ( 'NONE', #16292, #16331, #13200, .T. ) ;
#15002 = ORIENTED_EDGE ( 'NONE', *, *, #20614, .F. ) ;
#15003 = CARTESIAN_POINT ( 'NONE',  ( 4.165266963751720120, -4.099263933824012440, -2.757781224018043175E-14 ) ) ;
#15004 = EDGE_CURVE ( 'NONE', #4543, #22761, #15806, .T. ) ;
#15005 = CARTESIAN_POINT ( 'NONE',  ( -1.110223024625156540E-13, 1.999999999999932498, 7.500000000000034639 ) ) ;
#15006 = DIRECTION ( 'NONE',  ( 1.000000000000000000, 2.220446049250313081E-16, 4.712618736834399899E-47 ) ) ;
#15007 = DIRECTION ( 'NONE',  ( -1.000000000000000000, 0.000000000000000000, -1.066687855278535322E-26 ) ) ;
#15008 = CARTESIAN_POINT ( 'NONE',  ( -8.697224362267972353, -12.00000000000004619, 6.250000000000038192 ) ) ;
#15009 = CARTESIAN_POINT ( 'NONE',  ( -8.954763739086862628, -13.50000000000004086, 6.678571428571458135 ) ) ;
#15010 = DIRECTION ( 'NONE',  ( 2.013525853228507892E-32, 6.902532920683810383E-31, -1.000000000000000000 ) ) ;
#15011 = AXIS2_PLACEMENT_3D ( 'NONE', #5245, #21006, #21124 ) ;
#15012 = PLANE ( 'NONE',  #2381 ) ;
#15013 = PLANE ( 'NONE',  #1738 ) ;
#15014 = FACE_BOUND ( 'NONE', #20997, .T. ) ;
#15015 = FACE_OUTER_BOUND ( 'NONE', #1965, .T. ) ;
#15016 = ORIENTED_EDGE ( 'NONE', *, *, #2183, .T. ) ;
#15017 = ORIENTED_EDGE ( 'NONE', *, *, #19933, .T. ) ;
#15018 = ORIENTED_EDGE ( 'NONE', *, *, #12539, .T. ) ;
#15019 = VERTEX_POINT ( 'NONE', #18087 ) ;
#15020 = CARTESIAN_POINT ( 'NONE',  ( 12.84999999999997300, -12.00000000000002842, 5.750000000000018652 ) ) ;
#15021 = DIRECTION ( 'NONE',  ( -0.7071067811865412445, 0.7071067811865539010, 1.565905175853772837E-16 ) ) ;
#15022 = ORIENTED_EDGE ( 'NONE', *, *, #15156, .F. ) ;
#15023 = AXIS2_PLACEMENT_3D ( 'NONE', #155, #7327, #10943 ) ;
#15024 = DIRECTION ( 'NONE',  ( 1.000000000000000000, 3.254448077276381206E-32, 1.066788928082016908E-26 ) ) ;
#15025 = ADVANCED_FACE ( 'NONE', ( #8801 ), #1951, .F. ) ;
#15026 = LINE ( 'NONE', #7517, #5508 ) ;
#15027 = CARTESIAN_POINT ( 'NONE',  ( 8.502135871254301591, -0.5075717384767749474, 6.995667647939175282 ) ) ;
#15028 = CARTESIAN_POINT ( 'NONE',  ( -10.49999999999999467, -14.00000000000000888, 9.250000000000035527 ) ) ;
#15029 = EDGE_CURVE ( 'NONE', #9714, #7030, #16956, .T. ) ;
#15030 = DIRECTION ( 'NONE',  ( -1.066788928082016908E-26, -3.471809175856251779E-58, 1.000000000000000000 ) ) ;
#15031 = DIRECTION ( 'NONE',  ( -1.000000000000000000, -1.479114197289397135E-31, -5.916456789157588541E-31 ) ) ;
#15032 = CARTESIAN_POINT ( 'NONE',  ( -10.49999999999999467, -6.938893903907228378E-15, 6.250000000000005329 ) ) ;
#15033 = ADVANCED_FACE ( 'NONE', ( #3502 ), #12904, .T. ) ;
#15034 = CARTESIAN_POINT ( 'NONE',  ( -64.00000000000045475, -7.632783294297951215E-14, -2.000000000000001776 ) ) ;
#15035 = CARTESIAN_POINT ( 'NONE',  ( 8.204963667274169481, -13.91374178095067649, 7.312308861539038141 ) ) ;
#15036 = DIRECTION ( 'NONE',  ( 0.000000000000000000, 0.5000000000000026645, 0.8660254037844372643 ) ) ;
#15037 = DIRECTION ( 'NONE',  ( -1.000000000000000000, 0.000000000000000000, -4.336808689941968432E-16 ) ) ;
#15038 = CARTESIAN_POINT ( 'NONE',  ( 4.093692494532772841, 2.021783646005771207, -3.501831996793843160 ) ) ;
#15039 = AXIS2_PLACEMENT_3D ( 'NONE', #17797, #1678, #3218 ) ;
#15040 = VERTEX_POINT ( 'NONE', #7043 ) ;
#15041 = B_SPLINE_CURVE_WITH_KNOTS ( 'NONE', 3,
 ( #8071, #22424, #7725, #6316, #11474, #13489, #2426, #17111, #20672, #4537, #5971, #2780, #673, #7842, #21012, #11831 ),
 .UNSPECIFIED., .F., .F.,
 ( 4, 3, 3, 3, 3, 4 ),
 ( 0.000000000000000000, 3.315506744709155554E-05, 6.608280158698816038E-05, 0.0001026520855291328406, 0.0001376952025664795836, 0.0001398064759190610195 ),
 .UNSPECIFIED. ) ;
#15042 = EDGE_LOOP ( 'NONE', ( #14601, #15824, #3948, #18943 ) ) ;
#15044 = ORIENTED_EDGE ( 'NONE', *, *, #12498, .T. ) ;
#15043 = ORIENTED_EDGE ( 'NONE', *, *, #20821, .F. ) ;
#15045 = ADVANCED_BREP_SHAPE_REPRESENTATION ( '', ( #5304, #22115 ), #12708 ) ;
#15046 = CARTESIAN_POINT ( 'NONE',  ( -0.02511973781853877458, 4.877415612947472390, -3.751298745799859891 ) ) ;
#15047 = DIRECTION ( 'NONE',  ( -8.438582421954110511E-32, 0.000000000000000000, -1.000000000000000000 ) ) ;
#15048 = CARTESIAN_POINT ( 'NONE',  ( -3.499999999708153453, 35.99999999900384751, -18.50000000000000355 ) ) ;
#15049 = AXIS2_PLACEMENT_3D ( 'NONE', #3647, #5651, #21430 ) ;
#15050 = AXIS2_PLACEMENT_3D ( 'NONE', #13723, #17703, #23011 ) ;
#15051 = CARTESIAN_POINT ( 'NONE',  ( -3.499999999708153453, 42.99999999900385461, -26.00000000000000000 ) ) ;
#15052 = LINE ( 'NONE', #22244, #4897 ) ;
#15053 = CARTESIAN_POINT ( 'NONE',  ( 4.142654963991856398, -2.035398498734349193, 3.525413613457312412 ) ) ;
#15054 = CARTESIAN_POINT ( 'NONE',  ( -3.225797924675914696E-14, -0.5999999999999898748, 3.226849613583673282 ) ) ;
#15055 = DIRECTION ( 'NONE',  ( 0.000000000000000000, 0.000000000000000000, 1.000000000000000000 ) ) ;
#15056 = CARTESIAN_POINT ( 'NONE',  ( -45.56568542494957086, 2.108831175456883589, 7.500000000000047962 ) ) ;
#15057 = CARTESIAN_POINT ( 'NONE',  ( -2.000000000000015543, 3.464101615137746837, 0.000000000000000000 ) ) ;
#15058 =( NAMED_UNIT ( * ) SI_UNIT ( $, .STERADIAN. ) SOLID_ANGLE_UNIT ( ) );
#15059 = DIRECTION ( 'NONE',  ( -3.254448077146059901E-32, -1.000000000000000000, 6.656013887802287108E-31 ) ) ;
#15060 = FACE_BOUND ( 'NONE', #3687, .T. ) ;
#15061 = LINE ( 'NONE', #506, #12300 ) ;
#15062 = CARTESIAN_POINT ( 'NONE',  ( 4.690415759823637565, -0.7499999999999382716, -2.000000000000029310 ) ) ;
#15063 = DIRECTION ( 'NONE',  ( -0.7453559924999295649, 0.000000000000000000, 0.6666666666666669627 ) ) ;
#15064 = ORIENTED_EDGE ( 'NONE', *, *, #21051, .F. ) ;
#15065 = EDGE_CURVE ( 'NONE', #15111, #19572, #4931, .T. ) ;
#15066 = AXIS2_PLACEMENT_3D ( 'NONE', #19964, #12551, #18208 ) ;
#15068 = ORIENTED_EDGE ( 'NONE', *, *, #3043, .T. ) ;
#15067 = ORIENTED_EDGE ( 'NONE', *, *, #13004, .T. ) ;
#15069 = EDGE_LOOP ( 'NONE', ( #12177, #17815, #11786, #22335 ) ) ;
#15070 = EDGE_LOOP ( 'NONE', ( #2589, #513, #12528, #2181 ) ) ;
#15072 = ORIENTED_EDGE ( 'NONE', *, *, #9948, .F. ) ;
#15071 = VERTEX_POINT ( 'NONE', #16185 ) ;
#15073 = CARTESIAN_POINT ( 'NONE',  ( 0.000000000000000000, 0.000000000000000000, 0.000000000000000000 ) ) ;
#15074 = DIRECTION ( 'NONE',  ( -0.7071067811865539010, -0.7071067811865413555, 0.000000000000000000 ) ) ;
#15075 = ORIENTED_EDGE ( 'NONE', *, *, #10734, .T. ) ;
#15076 = CARTESIAN_POINT ( 'NONE',  ( 2.918498775983380256E-10, 36.49999999900384751, -25.50000000000000000 ) ) ;
#15077 = DIRECTION ( 'NONE',  ( 1.000000000000000000, 2.699383410053119644E-30, 3.330669073875432643E-16 ) ) ;
#15078 = CARTESIAN_POINT ( 'NONE',  ( 37.00000000000014211, 11.00000000000000000, -3.000000000000002665 ) ) ;
#15079 = APPLICATION_CONTEXT ( 'automotive_design' ) ;
#15080 = LINE ( 'NONE', #13686, #13160 ) ;
#15081 = CARTESIAN_POINT ( 'NONE',  ( -7.499999999999987566, -3.018576030000264421, 8.916666666666682062 ) ) ;
#15082 = CARTESIAN_POINT ( 'NONE',  ( 108.2426266706970353, -13.52760560296359316, -6.000000000000019540 ) ) ;
#15083 = CARTESIAN_POINT ( 'NONE',  ( 7.523705677365597921, -2.838350495275038909, 8.715168381933271036 ) ) ;
#15084 = AXIS2_PLACEMENT_3D ( 'NONE', #9726, #20433, #16759 ) ;
#15085 = AXIS2_PLACEMENT_3D ( 'NONE', #13163, #7158, #14318 ) ;
#15086 = CARTESIAN_POINT ( 'NONE',  ( 6.000000000291855429, 2.999999999003851503, -5.999999999999998224 ) ) ;
#15087 = ADVANCED_FACE ( 'NONE', ( #8914 ), #21120, .T. ) ;
#15088 = DIRECTION ( 'NONE',  ( 0.000000000000000000, 1.000000000000000000, 0.000000000000000000 ) ) ;
#15089 = DIRECTION ( 'NONE',  ( -1.000000000000000000, 0.000000000000000000, 0.000000000000000000 ) ) ;
#15090 = DIRECTION ( 'NONE',  ( -1.000000000000000000, -2.699383410053121045E-30, -3.717264591378832268E-16 ) ) ;
#15091 = PLANE ( 'NONE',  #22048 ) ;
#15092 = VERTEX_POINT ( 'NONE', #15229 ) ;
#15093 = EDGE_CURVE ( 'NONE', #8753, #21236, #22971, .T. ) ;
#15094 = COLOUR_RGB ( '', 0.40784314, 0.44705882, 0.49803922) ;
#15095 = SURFACE_SIDE_STYLE ('',( #6526 ) ) ;
#15097 = ORIENTED_EDGE ( 'NONE', *, *, #16391, .F. ) ;
#15096 = EDGE_LOOP ( 'NONE', ( #6322, #2153, #2041, #28, #22949, #16376 ) ) ;
#15098 = ORIENTED_EDGE ( 'NONE', *, *, #13532, .T. ) ;
#15099 = EDGE_CURVE ( 'NONE', #4862, #12385, #2686, .T. ) ;
#15100 = ORIENTED_EDGE ( 'NONE', *, *, #5701, .F. ) ;
#15101 = CIRCLE ( 'NONE', #13987, 5.500000000000033751 ) ;
#15102 = EDGE_CURVE ( 'NONE', #15655, #10116, #15116, .T. ) ;
#15103 = ORIENTED_EDGE ( 'NONE', *, *, #3528, .F. ) ;
#15104 = VECTOR ( 'NONE', #21507, 1000.000000000000000 ) ;
#15105 = ADVANCED_FACE ( 'NONE', ( #14781 ), #13248, .T. ) ;
#15106 = CIRCLE ( 'NONE', #463, 5.749999999999992006 ) ;
#15107 = B_SPLINE_CURVE_WITH_KNOTS ( 'NONE', 3,
 ( #8626, #15787, #21103, #22986, #6866, #22754, #1230, #17208, #14040, #11914, #21233, #20989, #11806, #18991, #15443, #12254 ),
 .UNSPECIFIED., .F., .F.,
 ( 4, 2, 2, 2, 2, 2, 2, 4 ),
 ( 0.000000000000000000, 0.0008458391445145495551, 0.001268758716771825742, 0.001691678289029102146, 0.002114597861286379200, 0.002537517433543656688, 0.002960437005800934177, 0.003383356578058211665 ),
 .UNSPECIFIED. ) ;
#15108 = ORIENTED_EDGE ( 'NONE', *, *, #15978, .F. ) ;
#15109 = CARTESIAN_POINT ( 'NONE',  ( 37.00000000000014211, 0.5000000000000004441, -3.000000000000002665 ) ) ;
#15110 = DIRECTION ( 'NONE',  ( -0.000000000000000000, -0.000000000000000000, 1.000000000000000000 ) ) ;
#15111 = VERTEX_POINT ( 'NONE', #22193 ) ;
#15112 = CARTESIAN_POINT ( 'NONE',  ( 4.114405500665258231, -4.051151509359430136, -3.718102049540426238E-17 ) ) ;
#15113 = AXIS2_PLACEMENT_3D ( 'NONE', #23226, #7113, #1795 ) ;
#15114 = CARTESIAN_POINT ( 'NONE',  ( 4.093692494532772841, 2.021783646005722801, 3.501831996793851154 ) ) ;
#15115 = CYLINDRICAL_SURFACE ( 'NONE', #9344, 7.000000000000075495 ) ;
#15116 = LINE ( 'NONE', #6199, #4946 ) ;
#15117 = CARTESIAN_POINT ( 'NONE',  ( -7.324400034341879362, -11.76702354778241499, 7.601326208249701288 ) ) ;
#15118 = EDGE_CURVE ( 'NONE', #800, #4569, #13951, .T. ) ;
#15119 = EDGE_CURVE ( 'NONE', #12006, #7483, #17258, .T. ) ;
#15120 = CARTESIAN_POINT ( 'NONE',  ( -7.748687480237919090, -13.73110298228156978, 8.040801957829067703 ) ) ;
#15121 = ADVANCED_FACE ( 'NONE', ( #16989 ), #18427, .T. ) ;
#15122 = CARTESIAN_POINT ( 'NONE',  ( -43.10883117545713361, -4.565685424949276872, 8.000000000000035527 ) ) ;
#15123 = AXIS2_PLACEMENT_3D ( 'NONE', #19012, #2886, #10066 ) ;
#15124 = CARTESIAN_POINT ( 'NONE',  ( 0.3126073911696447549, 4.041451884327383226, 0.000000000000000000 ) ) ;
#15125 = B_SPLINE_CURVE_WITH_KNOTS ( 'NONE', 3,
 ( #12108, #8483, #22839, #18833 ),
 .UNSPECIFIED., .F., .F.,
 ( 4, 4 ),
 ( 2.380737581730922818E-07, 0.002336974151641528670 ),
 .UNSPECIFIED. ) ;
#15126 = AXIS2_PLACEMENT_3D ( 'NONE', #12274, #14174, #3006 ) ;
#15127 = DIRECTION ( 'NONE',  ( -1.734723475976809806E-16, -1.000000000000000000, 0.000000000000000000 ) ) ;
#15128 = TOROIDAL_SURFACE ( 'NONE', #6881, 2.250000000000000444, 0.2500000000000000000 ) ;
#15129 = AXIS2_PLACEMENT_3D ( 'NONE', #17071, #22391, #15315 ) ;
#15130 = LINE ( 'NONE', #22323, #4441 ) ;
#15131 = FACE_BOUND ( 'NONE', #7691, .T. ) ;
#15132 = ORIENTED_EDGE ( 'NONE', *, *, #21956, .T. ) ;
#15133 = EDGE_CURVE ( 'NONE', #13324, #800, #2305, .T. ) ;
#15134 = ADVANCED_FACE ( 'NONE', ( #11473 ), #2539, .T. ) ;
#15135 = ORIENTED_EDGE ( 'NONE', *, *, #6959, .T. ) ;
#15136 = ORIENTED_EDGE ( 'NONE', *, *, #11228, .F. ) ;
#15137 = ADVANCED_FACE ( 'NONE', ( #6076 ), #16880, .T. ) ;
#15138 = EDGE_LOOP ( 'NONE', ( #3911, #2849, #21808, #16696 ) ) ;
#15139 = CARTESIAN_POINT ( 'NONE',  ( 3.806834918298644954, 3.031088913245544969, 1.750000000000003331 ) ) ;
#15140 = DIRECTION ( 'NONE',  ( 3.330669073875454830E-16, 0.000000000000000000, -1.000000000000000000 ) ) ;
#15141 = AXIS2_PLACEMENT_3D ( 'NONE', #23049, #10451, #8807 ) ;
#15142 = ORIENTED_EDGE ( 'NONE', *, *, #23203, .T. ) ;
#15143 = VECTOR ( 'NONE', #9431, 1000.000000000000000 ) ;
#15144 = CARTESIAN_POINT ( 'NONE',  ( 25.60000000000000142, 2.516649172247813527E-16, -2.055000000000009486 ) ) ;
#15145 = AXIS2_PLACEMENT_3D ( 'NONE', #7921, #8589, #20287 ) ;
#15146 = AXIS2_PLACEMENT_3D ( 'NONE', #1898, #19913, #7553 ) ;
#15147 = DIRECTION ( 'NONE',  ( -1.733449886265891589E-32, 4.190823558986610327E-31, -1.000000000000000000 ) ) ;
#15148 = CARTESIAN_POINT ( 'NONE',  ( -42.54314575050796776, 4.799999999999991829, -8.000000000000035527 ) ) ;
#15149 = VECTOR ( 'NONE', #8610, 1000.000000000000000 ) ;
#15150 =( GEOMETRIC_REPRESENTATION_CONTEXT ( 3 ) GLOBAL_UNCERTAINTY_ASSIGNED_CONTEXT ( ( #5579 ) ) GLOBAL_UNIT_ASSIGNED_CONTEXT ( ( #6129, #6015, #6366 ) ) REPRESENTATION_CONTEXT ( 'NONE', 'WORKASPACE' ) );
#15151 = CARTESIAN_POINT ( 'NONE',  ( -4.904729001344796835, 35.99999999900385461, -19.07709762542843634 ) ) ;
#15152 = CYLINDRICAL_SURFACE ( 'NONE', #20593, 2.099999999999999645 ) ;
#15153 = CARTESIAN_POINT ( 'NONE',  ( 4.296135882448235854, 0.7500000000000558442, -2.802242829034434557 ) ) ;
#15154 = DIRECTION ( 'NONE',  ( -3.070652698126927723E-17, -1.000000000000000000, 4.167305704548413124E-17 ) ) ;
#15155 = LINE ( 'NONE', #4449, #2449 ) ;
#15156 = EDGE_CURVE ( 'NONE', #14530, #10470, #6458, .T. ) ;
#15157 = CARTESIAN_POINT ( 'NONE',  ( -3.999999999708153453, 35.99999999900384751, -25.50000000000000000 ) ) ;
#15158 = CARTESIAN_POINT ( 'NONE',  ( -5.051814855409225480, 4.882486540518908846, -6.249999999999975131 ) ) ;
#15159 = LINE ( 'NONE', #22462, #16042 ) ;
#15160 = CARTESIAN_POINT ( 'NONE',  ( 124.5000000000019469, -13.52760560296373171, -6.938893903907228378E-15 ) ) ;
#15161 = AXIS2_PLACEMENT_3D ( 'NONE', #21606, #18070, #9237 ) ;
#15162 = CARTESIAN_POINT ( 'NONE',  ( 4.175813232069142344, 2.061359961916364725, -3.570380186727397209 ) ) ;
#15163 = AXIS2_PLACEMENT_3D ( 'NONE', #11044, #2454, #5879 ) ;
#15165 = VERTEX_POINT ( 'NONE', #2657 ) ;
#15164 = AXIS2_PLACEMENT_3D ( 'NONE', #3979, #20337, #4201 ) ;
#15166 = EDGE_CURVE ( 'NONE', #10359, #20148, #10937, .T. ) ;
#15167 = AXIS2_PLACEMENT_3D ( 'NONE', #14912, #5755, #19871 ) ;
#15168 = VERTEX_POINT ( 'NONE', #20671 ) ;
#15170 = ORIENTED_EDGE ( 'NONE', *, *, #19046, .F. ) ;
#15169 = ORIENTED_EDGE ( 'NONE', *, *, #15556, .T. ) ;
#15171 = DIRECTION ( 'NONE',  ( -4.440892098500626162E-15, 0.000000000000000000, 1.000000000000000000 ) ) ;
#15172 = ORIENTED_EDGE ( 'NONE', *, *, #6172, .T. ) ;
#15173 = AXIS2_PLACEMENT_3D ( 'NONE', #15560, #12020, #17083 ) ;
#15174 = CARTESIAN_POINT ( 'NONE',  ( -4.294683695178314942, -0.7499999999999437117, -2.803608044185096126 ) ) ;
#15175 = DIRECTION ( 'NONE',  ( 5.551115123561405253E-17, 1.000000000000000000, 2.256980353643891447E-27 ) ) ;
#15176 = VECTOR ( 'NONE', #1703, 1000.000000000000000 ) ;
#15177 = CARTESIAN_POINT ( 'NONE',  ( -8.326672684688674053E-14, 4.999999999999893419, 7.499999999999958256 ) ) ;
#15178 = CARTESIAN_POINT ( 'NONE',  ( 4.175813232069142344, -4.122719923832743660, 0.000000000000000000 ) ) ;
#15179 = CARTESIAN_POINT ( 'NONE',  ( 8.697224362267997222, -14.00000000000004974, 6.250000000000033751 ) ) ;
#15180 = CARTESIAN_POINT ( 'NONE',  ( 113.0166151911346475, -11.64708151429785765, -6.000000000000012434 ) ) ;
#15181 = DIRECTION ( 'NONE',  ( 0.000000000000000000, 0.000000000000000000, 1.000000000000000000 ) ) ;
#15182 = CARTESIAN_POINT ( 'NONE',  ( 22.49999999999998224, 2.000000000000001776, -2.081668171172168513E-14 ) ) ;
#15183 = EDGE_CURVE ( 'NONE', #280, #6091, #9378, .T. ) ;
#15184 = SURFACE_SIDE_STYLE ('',( #16935 ) ) ;
#15185 = CARTESIAN_POINT ( 'NONE',  ( -50.65685424949280247, -0.5000000000001045830, 7.500000000000062172 ) ) ;
#15186 = DIRECTION ( 'NONE',  ( -1.734723475976813750E-16, -1.000000000000000000, 3.469446951953607484E-15 ) ) ;
#15187 = ADVANCED_FACE ( 'NONE', ( #22077 ), #22606, .T. ) ;
#15188 = ORIENTED_EDGE ( 'NONE', *, *, #21882, .T. ) ;
#15189 = VECTOR ( 'NONE', #22720, 1000.000000000000000 ) ;
#15191 = ORIENTED_EDGE ( 'NONE', *, *, #22114, .T. ) ;
#15190 = VERTEX_POINT ( 'NONE', #2193 ) ;
#15192 = UNCERTAINTY_MEASURE_WITH_UNIT (LENGTH_MEASURE( 1.000000000000000082E-05 ), #3135, 'distance_accuracy_value', 'NONE');
#15193 = EDGE_CURVE ( 'NONE', #20913, #8586, #19222, .T. ) ;
#15194 = ORIENTED_EDGE ( 'NONE', *, *, #6779, .F. ) ;
#15196 = VERTEX_POINT ( 'NONE', #5857 ) ;
#15195 = ORIENTED_EDGE ( 'NONE', *, *, #20885, .F. ) ;
#15197 = ORIENTED_EDGE ( 'NONE', *, *, #14592, .T. ) ;
#15198 = CARTESIAN_POINT ( 'NONE',  ( -42.54314575050778302, -7.500000000000020428, 7.500000000000034639 ) ) ;
#15199 = DIRECTION ( 'NONE',  ( -1.000000000000000000, 0.000000000000000000, 0.000000000000000000 ) ) ;
#15200 = EDGE_LOOP ( 'NONE', ( #1833, #21859, #22409, #11083 ) ) ;
#15201 = DIRECTION ( 'NONE',  ( 3.330669073875432643E-16, 4.437342591868153746E-31, -1.000000000000000000 ) ) ;
#15202 = CARTESIAN_POINT ( 'NONE',  ( 0.000000000000000000, 0.000000000000000000, -3.499999999999996003 ) ) ;
#15203 = FACE_OUTER_BOUND ( 'NONE', #19807, .T. ) ;
#15204 = CARTESIAN_POINT ( 'NONE',  ( -7.467942433933805191, -2.153931645084739444, 7.356484134531028118 ) ) ;
#15205 = CARTESIAN_POINT ( 'NONE',  ( 4.197310751797331818, 0.8178363989515984311, -3.502498386812460840 ) ) ;
#15206 = CARTESIAN_POINT ( 'NONE',  ( 7.971461718369192262, -2.232205167193722861, 7.625732677302370810 ) ) ;
#15207 = CYLINDRICAL_SURFACE ( 'NONE', #17424, 2.549999999999997158 ) ;
#15208 = CARTESIAN_POINT ( 'NONE',  ( -3.499999999708153453, 2.999999999003851503, -26.50000000000000000 ) ) ;
#15209 = CARTESIAN_POINT ( 'NONE',  ( 4.163336342344337027E-14, 3.469446951953614189E-14, -3.000000000000002665 ) ) ;
#15210 = DIRECTION ( 'NONE',  ( 1.000000000000000000, -1.847414967615758933E-47, 3.885780586188017323E-16 ) ) ;
#15211 = DIRECTION ( 'NONE',  ( 0.8191520442889933529, -1.029921702463443268E-15, 0.5735764363510438280 ) ) ;
#15212 = DIRECTION ( 'NONE',  ( -0.8191520442889939080, 1.162110848990233300E-15, 0.5735764363510431618 ) ) ;
#15213 = EDGE_LOOP ( 'NONE', ( #14251, #7200, #22091, #16299 ) ) ;
#15214 = UNCERTAINTY_MEASURE_WITH_UNIT (LENGTH_MEASURE( 1.000000000000000082E-05 ), #12260, 'distance_accuracy_value', 'NONE');
#15216 = ORIENTED_EDGE ( 'NONE', *, *, #19333, .T. ) ;
#15215 = ORIENTED_EDGE ( 'NONE', *, *, #21476, .F. ) ;
#15217 = ORIENTED_EDGE ( 'NONE', *, *, #2987, .F. ) ;
#15218 = ORIENTED_EDGE ( 'NONE', *, *, #10553, .F. ) ;
#15219 = ORIENTED_EDGE ( 'NONE', *, *, #11027, .T. ) ;
#15220 = PRODUCT_DEFINITION ( 'UNKNOWN', '', #11621, #20881 ) ;
#15221 = ORIENTED_EDGE ( 'NONE', *, *, #14408, .T. ) ;
#15222 = CARTESIAN_POINT ( 'NONE',  ( -7.500000000000034639, -12.60977222864646485, 9.250000000000063949 ) ) ;
#15223 = CYLINDRICAL_SURFACE ( 'NONE', #19261, 2.549999999999996714 ) ;
#15224 = EDGE_LOOP ( 'NONE', ( #16262, #4554, #22733, #7797 ) ) ;
#15225 = DIRECTION ( 'NONE',  ( -2.887593071917436153E-31, -7.888609052210128564E-31, 1.000000000000000000 ) ) ;
#15226 = ADVANCED_FACE ( 'NONE', ( #21129 ), #12455, .T. ) ;
#15227 = DIRECTION ( 'NONE',  ( 0.000000000000000000, -1.000000000000000000, 0.000000000000000000 ) ) ;
#15228 = CARTESIAN_POINT ( 'NONE',  ( 0.000000000000000000, 0.000000000000000000, -5.574599999999999334 ) ) ;
#15229 = CARTESIAN_POINT ( 'NONE',  ( -43.10883117545713361, -4.565685424949256443, -7.500000000000007105 ) ) ;
#15230 = CARTESIAN_POINT ( 'NONE',  ( -7.835522544085319119, -11.94917567266013236, 6.894286109559293330 ) ) ;
#15231 = CARTESIAN_POINT ( 'NONE',  ( -8.148407558030072551, -13.43987109532831248, 7.382406087064029343 ) ) ;
#15232 = FACE_OUTER_BOUND ( 'NONE', #9137, .T. ) ;
#15233 = EDGE_CURVE ( 'NONE', #21954, #20178, #16940, .T. ) ;
#15234 = CARTESIAN_POINT ( 'NONE',  ( 0.2174200650117545097, 3.876582599186212619, 0.2855619784720683230 ) ) ;
#15235 = CARTESIAN_POINT ( 'NONE',  ( 124.5000000000017764, -4.500000000000003553, 6.000000000000116351 ) ) ;
#15236 = ORIENTED_EDGE ( 'NONE', *, *, #18281, .F. ) ;
#15237 = AXIS2_PLACEMENT_3D ( 'NONE', #21791, #16234, #21332 ) ;
#15238 =( NAMED_UNIT ( * ) PLANE_ANGLE_UNIT ( ) SI_UNIT ( $, .RADIAN. ) );
#15239 = CARTESIAN_POINT ( 'NONE',  ( 4.086376042167605860, 4.082715877136870120, -0.07147133206917886949 ) ) ;
#15240 = LINE ( 'NONE', #13731, #12291 ) ;
#15241 = ORIENTED_EDGE ( 'NONE', *, *, #14388, .T. ) ;
#15242 = ADVANCED_FACE ( 'NONE', ( #6654 ), #6827, .T. ) ;
#15243 = AXIS2_PLACEMENT_3D ( 'NONE', #10109, #20936, #3048 ) ;
#15244 = VERTEX_POINT ( 'NONE', #22545 ) ;
#15245 = ORIENTED_EDGE ( 'NONE', *, *, #18700, .F. ) ;
#15246 = VERTEX_POINT ( 'NONE', #4765 ) ;
#15247 = ORIENTED_EDGE ( 'NONE', *, *, #20560, .T. ) ;
#15248 = DIRECTION ( 'NONE',  ( 0.1556420233463076119, 0.000000000000000000, 0.9878135252003121813 ) ) ;
#15249 = EDGE_CURVE ( 'NONE', #7483, #18303, #3132, .T. ) ;
#15250 = FACE_OUTER_BOUND ( 'NONE', #21469, .T. ) ;
#15251 = VERTEX_POINT ( 'NONE', #22777 ) ;
#15252 = CIRCLE ( 'NONE', #8500, 2.549999999999997158 ) ;
#15253 = FACE_OUTER_BOUND ( 'NONE', #8550, .T. ) ;
#15254 = CARTESIAN_POINT ( 'NONE',  ( 54.42435809754106657, -4.000000000000003553, 6.000000000000136779 ) ) ;
#15255 = DIRECTION ( 'NONE',  ( -0.000000000000000000, -0.000000000000000000, 1.000000000000000000 ) ) ;
#15256 = EDGE_CURVE ( 'NONE', #15655, #7223, #11697, .T. ) ;
#15257 = CARTESIAN_POINT ( 'NONE',  ( 42.50000000000014921, 8.000000000000003553, -12.49999999999998401 ) ) ;
#15258 = CARTESIAN_POINT ( 'NONE',  ( 12.84999999999999964, -13.50000000000011191, -6.249999999999936051 ) ) ;
#15259 = DIRECTION ( 'NONE',  ( 0.000000000000000000, 0.000000000000000000, 1.000000000000000000 ) ) ;
#15260 = DIRECTION ( 'NONE',  ( 0.000000000000000000, 0.000000000000000000, -1.000000000000000000 ) ) ;
#15261 = VECTOR ( 'NONE', #9967, 1000.000000000000000 ) ;
#15262 = LINE ( 'NONE', #13286, #11075 ) ;
#15263 = ADVANCED_FACE ( 'NONE', ( #8192 ), #4878, .T. ) ;
#15264 = STYLED_ITEM ( 'NONE', ( #16506 ), #5146 ) ;
#15265 = EDGE_CURVE ( 'NONE', #7940, #21726, #16085, .T. ) ;
#15266 = CARTESIAN_POINT ( 'NONE',  ( 0.1217565302851057185, -2.351289329882179757, -2.927447417349501979 ) ) ;
#15267 = DIRECTION ( 'NONE',  ( -1.000000000000000000, -4.252453317207022018E-31, 5.551115123125818447E-17 ) ) ;
#15269 = ADVANCED_FACE ( 'NONE', ( #19233 ), #19973, .T. ) ;
#15268 = CARTESIAN_POINT ( 'NONE',  ( -4.000000000000100364, 2.309401076758546445, -3.433295621305381573 ) ) ;
#15270 = CARTESIAN_POINT ( 'NONE',  ( -3.680118525130293250, 2.494084732383297531, -0.3507732604232518536 ) ) ;
#15271 = AXIS2_PLACEMENT_3D ( 'NONE', #9861, #935, #8093 ) ;
#15272 = CONTEXT_DEPENDENT_SHAPE_REPRESENTATION ( #20824, #15673 ) ;
#15273 = ORIENTED_EDGE ( 'NONE', *, *, #11667, .T. ) ;
#15274 = EDGE_CURVE ( 'NONE', #11922, #8762, #14342, .T. ) ;
#15275 = EDGE_CURVE ( 'NONE', #19106, #11464, #2779, .T. ) ;
#15276 = AXIS2_PLACEMENT_3D ( 'NONE', #16713, #20375, #11539 ) ;
#15277 = ADVANCED_FACE ( 'NONE', ( #13939 ), #11327, .T. ) ;
#15278 = ADVANCED_FACE ( 'NONE', ( #20791 ), #17335, .T. ) ;
#15279 = CIRCLE ( 'NONE', #15664, 0.5000000000000029976 ) ;
#15281 = ORIENTED_EDGE ( 'NONE', *, *, #8520, .F. ) ;
#15280 = EDGE_LOOP ( 'NONE', ( #5381, #2270, #11336, #747 ) ) ;
#15282 = DIRECTION ( 'NONE',  ( -9.693522803355793065E-26, 5.963788443470849249E-28, 1.000000000000000000 ) ) ;
#15283 = DIRECTION ( 'NONE',  ( 0.000000000000000000, -1.000000000000000000, 0.000000000000000000 ) ) ;
#15284 = DIRECTION ( 'NONE',  ( 1.000000000000000000, 0.000000000000000000, 1.066811114794976679E-26 ) ) ;
#15285 = AXIS2_PLACEMENT_3D ( 'NONE', #21409, #5510, #10681 ) ;
#15286 = VERTEX_POINT ( 'NONE', #4657 ) ;
#15287 = CARTESIAN_POINT ( 'NONE',  ( 3.649122391096873752, -1.701165921963298633, 3.179534615582995105 ) ) ;
#15288 = EDGE_CURVE ( 'NONE', #10662, #16835, #10580, .T. ) ;
#15289 = CARTESIAN_POINT ( 'NONE',  ( -2.428612866367529932E-14, 2.000000000000043521, -18.75000000000001066 ) ) ;
#15290 = PRODUCT_DEFINITION_SHAPE ( 'NONE', 'NONE',  #4448 ) ;
#15291 = LINE ( 'NONE', #8011, #6507 ) ;
#15292 = DIRECTION ( 'NONE',  ( -1.000000000000000000, 1.550910762415508562E-16, 0.000000000000000000 ) ) ;
#15293 = FACE_OUTER_BOUND ( 'NONE', #16639, .T. ) ;
#15294 = ADVANCED_FACE ( 'NONE', ( #23009 ), #18840, .T. ) ;
#15295 = CARTESIAN_POINT ( 'NONE',  ( -6.000000000000074607, 5.299999999999964295, 7.500000000000062172 ) ) ;
#15296 = CARTESIAN_POINT ( 'NONE',  ( -4.000000000000003553, -2.309401076758532678, -5.242734410091827613 ) ) ;
#15297 = CARTESIAN_POINT ( 'NONE',  ( 77.42435809754130105, -10.99999999999981526, 6.000000000000123457 ) ) ;
#15298 = CARTESIAN_POINT ( 'NONE',  ( 6.000000000291855429, 2.999999999003851503, -45.00000000000000000 ) ) ;
#15299 = AXIS2_PLACEMENT_3D ( 'NONE', #922, #4668, #22324 ) ;
#15300 = FACE_OUTER_BOUND ( 'NONE', #7715, .T. ) ;
#15301 = CARTESIAN_POINT ( 'NONE',  ( -50.65685424949273141, 0.5000000000000143219, 8.000000000000076383 ) ) ;
#15302 = AXIS2_PLACEMENT_3D ( 'NONE', #11385, #15031, #22220 ) ;
#15303 = LINE ( 'NONE', #4243, #1769 ) ;
#15304 = ORIENTED_EDGE ( 'NONE', *, *, #7206, .F. ) ;
#15305 = CIRCLE ( 'NONE', #3359, 0.5000000000000017764 ) ;
#15306 = CIRCLE ( 'NONE', #12693, 4.750000000000000888 ) ;
#15307 = CARTESIAN_POINT ( 'NONE',  ( 0.000000000000000000, 0.000000000000000000, 0.000000000000000000 ) ) ;
#15309 = EDGE_LOOP ( 'NONE', ( #22028, #17721, #10936, #22969 ) ) ;
#15308 = ORIENTED_EDGE ( 'NONE', *, *, #4981, .F. ) ;
#15310 = ORIENTED_EDGE ( 'NONE', *, *, #8521, .F. ) ;
#15312 = EDGE_LOOP ( 'NONE', ( #10058, #22024, #16488, #21926 ) ) ;
#15311 = ORIENTED_EDGE ( 'NONE', *, *, #8806, .T. ) ;
#15313 = VECTOR ( 'NONE', #5507, 1000.000000000000114 ) ;
#15314 = VERTEX_POINT ( 'NONE', #15467 ) ;
#15315 = DIRECTION ( 'NONE',  ( 0.000000000000000000, -1.734723475976807094E-15, -1.000000000000000000 ) ) ;
#15316 = VECTOR ( 'NONE', #1000, 1000.000000000000000 ) ;
#15317 = DIRECTION ( 'NONE',  ( -3.070652698126927723E-17, -1.000000000000000000, 4.167305704548413124E-17 ) ) ;
#15318 = ORIENTED_EDGE ( 'NONE', *, *, #15265, .F. ) ;
#15319 = SURFACE_SIDE_STYLE ('',( #8152 ) ) ;
#15320 = CARTESIAN_POINT ( 'NONE',  ( 0.02944718078427569982, -0.6813962075686340603, -3.500000000000010214 ) ) ;
#15321 = EDGE_CURVE ( 'NONE', #14050, #15515, #20355, .T. ) ;
#15322 = CARTESIAN_POINT ( 'NONE',  ( 0.4500000002918510544, 42.99999999900385461, -25.50000000000000355 ) ) ;
#15323 = LINE ( 'NONE', #6620, #1973 ) ;
#15324 = AXIS2_PLACEMENT_3D ( 'NONE', #11867, #13868, #19270 ) ;
#15325 = CYLINDRICAL_SURFACE ( 'NONE', #11429, 0.5000000000000037748 ) ;
#15326 = CARTESIAN_POINT ( 'NONE',  ( 3.999999999999619860, -1.677850389431014166, -3.535268758348135698 ) ) ;
#15327 = VECTOR ( 'NONE', #1764, 1000.000000000000000 ) ;
#15328 = CARTESIAN_POINT ( 'NONE',  ( 42.50000000000014921, 0.5000000000000004441, -12.49999999999998401 ) ) ;
#15329 = CARTESIAN_POINT ( 'NONE',  ( 4.086376210449949475, 2.103254844323304340, 3.499999999999996447 ) ) ;
#15330 = FACE_OUTER_BOUND ( 'NONE', #14911, .T. ) ;
#15331 = EDGE_CURVE ( 'NONE', #8906, #22878, #2130, .T. ) ;
#15332 = FACE_OUTER_BOUND ( 'NONE', #3388, .T. ) ;
#15333 = DIRECTION ( 'NONE',  ( 0.7071067811865505703, -0.7071067811865444641, -1.010793663541190129E-16 ) ) ;
#15334 = PLANE ( 'NONE',  #21718 ) ;
#15335 = CARTESIAN_POINT ( 'NONE',  ( 4.180345136606688605, -2.085999704580135727, -3.570468642550122862 ) ) ;
#15336 = ORIENTED_EDGE ( 'NONE', *, *, #7261, .F. ) ;
#15338 = ORIENTED_EDGE ( 'NONE', *, *, #10827, .F. ) ;
#15337 = ORIENTED_EDGE ( 'NONE', *, *, #3895, .T. ) ;
#15339 = VERTEX_POINT ( 'NONE', #385 ) ;
#15340 = CIRCLE ( 'NONE', #6339, 5.749999999999992006 ) ;
#15341 = ORIENTED_EDGE ( 'NONE', *, *, #2006, .T. ) ;
#15342 = B_SPLINE_CURVE_WITH_KNOTS ( 'NONE', 3,
 ( #11803, #13347, #12023, #18990, #6290, #10270 ),
 .UNSPECIFIED., .F., .F.,
 ( 4, 2, 4 ),
 ( 0.004120275011746843581, 0.005288420935197119671, 0.006456566858647396628 ),
 .UNSPECIFIED. ) ;
#15343 = CIRCLE ( 'NONE', #5159, 7.000000000000006217 ) ;
#15344 = AXIS2_PLACEMENT_3D ( 'NONE', #5711, #7582, #292 ) ;
#15345 = ORIENTED_EDGE ( 'NONE', *, *, #16611, .T. ) ;
#15346 = VERTEX_POINT ( 'NONE', #5682 ) ;
#15347 = CARTESIAN_POINT ( 'NONE',  ( 4.165266963751715679, -2.049631966912040415, 3.550066703508925059 ) ) ;
#15348 = DIRECTION ( 'NONE',  ( -0.6819983600624981435, -0.7313537016191709039, 0.000000000000000000 ) ) ;
#15349 = EDGE_LOOP ( 'NONE', ( #10525, #17517, #12448, #8179, #15486, #11122 ) ) ;
#15350 = PLANE ( 'NONE',  #5272 ) ;
#15351 = CARTESIAN_POINT ( 'NONE',  ( -89.70000000000048601, -3.200000000000105427, 1.000000000000000888 ) ) ;
#15352 = DIRECTION ( 'NONE',  ( 1.000000000000000000, 1.424116703980846297E-16, -1.095779650622964657E-32 ) ) ;
#15353 = CARTESIAN_POINT ( 'NONE',  ( 5.100000000000010303, 6.368163355566245256E-16, -5.200000000000001066 ) ) ;
#15354 = VECTOR ( 'NONE', #1415, 1000.000000000000000 ) ;
#15355 = DIRECTION ( 'NONE',  ( 1.000000000000000000, 2.220446049250313081E-16, -3.656342123407315983E-48 ) ) ;
#15356 = CARTESIAN_POINT ( 'NONE',  ( -7.120027569165209513, -11.54977705885991668, 8.099087005775032821 ) ) ;
#15357 = CARTESIAN_POINT ( 'NONE',  ( 124.5000000000019469, -6.500000000000061284, 4.857225732735059864E-14 ) ) ;
#15358 = CARTESIAN_POINT ( 'NONE',  ( -56.54644007500113645, 1.387778780781445676E-14, -8.666666666666710483 ) ) ;
#15359 = TOROIDAL_SURFACE ( 'NONE', #9749, 5.500000000000007994, 0.5000000000000000000 ) ;
#15360 = DIRECTION ( 'NONE',  ( 0.000000000000000000, 0.000000000000000000, 1.000000000000000000 ) ) ;
#15361 = LINE ( 'NONE', #22551, #14518 ) ;
#15362 = ORIENTED_EDGE ( 'NONE', *, *, #12133, .F. ) ;
#15363 = CARTESIAN_POINT ( 'NONE',  ( -5.560781378645589967, 7.794222813499895943E-15, -4.000000000000000000 ) ) ;
#15364 = CARTESIAN_POINT ( 'NONE',  ( 36.00000000029184832, 2.999999999003851503, -5.999999999999998224 ) ) ;
#15365 = VERTEX_POINT ( 'NONE', #21375 ) ;
#15366 = ADVANCED_FACE ( 'NONE', ( #11072 ), #9552, .F. ) ;
#15367 = ORIENTED_EDGE ( 'NONE', *, *, #8272, .T. ) ;
#15368 = VERTEX_POINT ( 'NONE', #12405 ) ;
#15369 = ORIENTED_EDGE ( 'NONE', *, *, #18026, .T. ) ;
#15370 = ORIENTED_EDGE ( 'NONE', *, *, #6771, .T. ) ;
#15371 = CARTESIAN_POINT ( 'NONE',  ( -4.000000000000003553, 1.935983797701083642, -5.350530693383765524 ) ) ;
#15372 = CIRCLE ( 'NONE', #11246, 4.500000000000045297 ) ;
#15373 = DIRECTION ( 'NONE',  ( -1.000000000000000000, 4.440892098500637995E-16, 0.000000000000000000 ) ) ;
#15374 = ORIENTED_EDGE ( 'NONE', *, *, #15397, .F. ) ;
#15375 = DIRECTION ( 'NONE',  ( 0.000000000000000000, 0.000000000000000000, -1.000000000000000000 ) ) ;
#15376 = DIRECTION ( 'NONE',  ( 1.000000000000000000, 0.000000000000000000, -0.000000000000000000 ) ) ;
#15377 = CARTESIAN_POINT ( 'NONE',  ( -6.866595637048056311, 0.5000000000001045830, 27.70872448147268585 ) ) ;
#15378 = CARTESIAN_POINT ( 'NONE',  ( 6.500000000000227374, 1.665334536937734811E-13, 6.000000000000213163 ) ) ;
#15379 = DIRECTION ( 'NONE',  ( -3.885780586188016830E-16, -4.437342591868156373E-31, 1.000000000000000000 ) ) ;
#15380 = CIRCLE ( 'NONE', #9001, 0.5000000000000038858 ) ;
#15381 = CARTESIAN_POINT ( 'NONE',  ( -7.029812747553701335, -0.6228290751909227874, 8.933015330925734077 ) ) ;
#15382 = AXIS2_PLACEMENT_3D ( 'NONE', #15648, #16110, #10361 ) ;
#15383 = CARTESIAN_POINT ( 'NONE',  ( -91.02295700146254376, -2.700000000000125855, 6.338518968055040226 ) ) ;
#15384 = CARTESIAN_POINT ( 'NONE',  ( 0.1217565302851110615, -3.710888496608917730, 0.5725525826504641591 ) ) ;
#15385 = FACE_OUTER_BOUND ( 'NONE', #14167, .T. ) ;
#15386 = CARTESIAN_POINT ( 'NONE',  ( 4.071447262713884463, 2.020725942163688504, 3.499999999999997780 ) ) ;
#15387 = DIRECTION ( 'NONE',  ( 3.032184104443272185E-30, 1.000000000000000000, -7.395570986447005381E-32 ) ) ;
#15388 = ADVANCED_FACE ( 'NONE', ( #22016 ), #12963, .T. ) ;
#15389 = DIRECTION ( 'NONE',  ( -1.000000000000000000, 4.190823558986610327E-31, -1.733449886265890494E-32 ) ) ;
#15390 = VERTEX_POINT ( 'NONE', #7441 ) ;
#15391 = EDGE_CURVE ( 'NONE', #1774, #15251, #13594, .T. ) ;
#15392 = AXIS2_PLACEMENT_3D ( 'NONE', #17464, #15691, #1364 ) ;
#15393 = ORIENTED_EDGE ( 'NONE', *, *, #17733, .F. ) ;
#15396 = ORIENTED_EDGE ( 'NONE', *, *, #16415, .F. ) ;
#15395 = EDGE_CURVE ( 'NONE', #1098, #16034, #90, .T. ) ;
#15394 = ORIENTED_EDGE ( 'NONE', *, *, #17181, .F. ) ;
#15397 = EDGE_CURVE ( 'NONE', #1072, #12423, #22266, .T. ) ;
#15398 = ORIENTED_EDGE ( 'NONE', *, *, #1360, .T. ) ;
#15399 = CARTESIAN_POINT ( 'NONE',  ( 3.000000000291852764, 42.99999999900385461, -15.99999999999999289 ) ) ;
#15400 = ADVANCED_FACE ( 'NONE', ( #14611 ), #4123, .T. ) ;
#15401 = CARTESIAN_POINT ( 'NONE',  ( -43.10883117545721888, 4.565685424949256443, -7.500000000000034639 ) ) ;
#15402 = CARTESIAN_POINT ( 'NONE',  ( 24.74999999999997513, 0.000000000000000000, -2.000000000000022649 ) ) ;
#15403 = ORIENTED_EDGE ( 'NONE', *, *, #19611, .T. ) ;
#15404 = DIRECTION ( 'NONE',  ( -1.000000000000000000, -1.479114197289388027E-30, 2.013525853228518840E-32 ) ) ;
#15405 = DIRECTION ( 'NONE',  ( 0.000000000000000000, 0.000000000000000000, 1.000000000000000000 ) ) ;
#15406 = CARTESIAN_POINT ( 'NONE',  ( 6.500000000000227374, 0.5000000000001669775, 6.000000000000213163 ) ) ;
#15407 = CARTESIAN_POINT ( 'NONE',  ( -4.499999999708154341, 35.49999999900384751, -19.50000000000000355 ) ) ;
#15408 = CARTESIAN_POINT ( 'NONE',  ( 2.344047193898538772, 3.265465875126504880, -2.077348303141170793E-15 ) ) ;
#15409 = CARTESIAN_POINT ( 'NONE',  ( -50.65685424949273141, 7.200000000000025935, 8.000000000000076383 ) ) ;
#15410 = CONICAL_SURFACE ( 'NONE', #9041, 3.499999999999999556, 1.047197551196600074 ) ;
#15411 = DIRECTION ( 'NONE',  ( -1.000000000000000000, 1.550910762415566494E-16, -8.566929763922626680E-48 ) ) ;
#15412 = LINE ( 'NONE', #22840, #7091 ) ;
#15413 = CARTESIAN_POINT ( 'NONE',  ( 0.000000000000000000, 0.000000000000000000, 0.000000000000000000 ) ) ;
#15414 = EDGE_CURVE ( 'NONE', #13674, #5698, #3081, .T. ) ;
#15415 = EDGE_CURVE ( 'NONE', #882, #20683, #19225, .T. ) ;
#15416 = CYLINDRICAL_SURFACE ( 'NONE', #22472, 2.499999999999990674 ) ;
#15417 = PLANE ( 'NONE',  #9333 ) ;
#15418 = LINE ( 'NONE', #8259, #7404 ) ;
#15419 = EDGE_LOOP ( 'NONE', ( #5467, #17820, #10509, #20859 ) ) ;
#15420 = CARTESIAN_POINT ( 'NONE',  ( -142.6487227650926286, 82.50018113422065369, 31.16570243528398620 ) ) ;
#15422 = EDGE_LOOP ( 'NONE', ( #7122, #10743, #13130, #11367 ) ) ;
#15421 = ORIENTED_EDGE ( 'NONE', *, *, #1399, .F. ) ;
#15423 = EDGE_CURVE ( 'NONE', #10146, #16829, #1589, .T. ) ;
#15424 = VERTEX_POINT ( 'NONE', #18144 ) ;
#15427 = ORIENTED_EDGE ( 'NONE', *, *, #10356, .T. ) ;
#15426 = EDGE_CURVE ( 'NONE', #5256, #13332, #18859, .T. ) ;
#15425 = EDGE_LOOP ( 'NONE', ( #2771, #12648, #17823, #20709 ) ) ;
#15428 = AXIS2_PLACEMENT_3D ( 'NONE', #15522, #22718, #6598 ) ;
#15429 = VERTEX_POINT ( 'NONE', #18482 ) ;
#15430 = CARTESIAN_POINT ( 'NONE',  ( 4.175813232069149450, 4.122719923832687705, 1.040834085586084257E-14 ) ) ;
#15431 = ADVANCED_FACE ( 'NONE', ( #12282 ), #5121, .T. ) ;
#15432 = CARTESIAN_POINT ( 'NONE',  ( -7.000000000000006217, -5.999999999999974243, 10.24999999999998224 ) ) ;
#15433 =( LENGTH_UNIT ( ) NAMED_UNIT ( * ) SI_UNIT ( .MILLI., .METRE. ) );
#15434 = CARTESIAN_POINT ( 'NONE',  ( 0.4500000002918510544, 42.99999999900385461, -19.00000000000000355 ) ) ;
#15435 = FACE_OUTER_BOUND ( 'NONE', #23056, .T. ) ;
#15436 = CARTESIAN_POINT ( 'NONE',  ( -7.734741761309916086, -2.069990213851658822, 7.004299047562754232 ) ) ;
#15437 = CARTESIAN_POINT ( 'NONE',  ( 88.75737332930594903, -13.52760560296348302, 6.000000000000130562 ) ) ;
#15438 = DIRECTION ( 'NONE',  ( -1.000000000000000000, 0.000000000000000000, 0.000000000000000000 ) ) ;
#15439 = CARTESIAN_POINT ( 'NONE',  ( 7.972478112619701740, -1.636497393431803893, 7.628219499134162085 ) ) ;
#15440 = CARTESIAN_POINT ( 'NONE',  ( 0.6920835326022192202, 4.454600218803903111, -3.597382984111570092 ) ) ;
#15441 = DIRECTION ( 'NONE',  ( -7.395570986446975166E-31, -3.382522293539642681E-32, -1.000000000000000000 ) ) ;
#15442 = DIRECTION ( 'NONE',  ( 1.000000000000000000, -4.440892098500658702E-16, 0.000000000000000000 ) ) ;
#15443 = CARTESIAN_POINT ( 'NONE',  ( -8.832214555408096857, -12.50000000000003908, 6.752214322824835691 ) ) ;
#15444 = AXIS2_PLACEMENT_3D ( 'NONE', #6454, #3165, #17617 ) ;
#15445 = AXIS2_PLACEMENT_3D ( 'NONE', #15357, #18780, #8073 ) ;
#15446 = CARTESIAN_POINT ( 'NONE',  ( -45.91923881554281195, -2.462384566050190848, -8.000000000000062172 ) ) ;
#15447 = CARTESIAN_POINT ( 'NONE',  ( 10.50000000000000888, -1.500000000000001332, 6.250000000000005329 ) ) ;
#15448 = ORIENTED_EDGE ( 'NONE', *, *, #7152, .T. ) ;
#15450 = EDGE_LOOP ( 'NONE', ( #14737, #22851 ) ) ;
#15449 = ORIENTED_EDGE ( 'NONE', *, *, #2788, .T. ) ;
#15451 = EDGE_CURVE ( 'NONE', #12056, #11543, #14840, .T. ) ;
#15452 = ORIENTED_EDGE ( 'NONE', *, *, #8393, .F. ) ;
#15453 = ORIENTED_EDGE ( 'NONE', *, *, #4199, .F. ) ;
#15454 = EDGE_LOOP ( 'NONE', ( #16567, #14282, #15750, #11523 ) ) ;
#15455 = EDGE_CURVE ( 'NONE', #6443, #13762, #2696, .T. ) ;
#15456 = ORIENTED_EDGE ( 'NONE', *, *, #6805, .T. ) ;
#15457 = CARTESIAN_POINT ( 'NONE',  ( 4.142654963991867056, -2.035398498734353190, 3.525413613457324402 ) ) ;
#15458 = AXIS2_PLACEMENT_3D ( 'NONE', #16645, #9838, #13488 ) ;
#15459 = CIRCLE ( 'NONE', #1204, 0.5000000000000024425 ) ;
#15460 = DIRECTION ( 'NONE',  ( 9.693522803355793065E-26, -5.963788443470848352E-28, -1.000000000000000000 ) ) ;
#15461 = EDGE_LOOP ( 'NONE', ( #15075, #15677, #20734, #20159 ) ) ;
#15462 = ORIENTED_EDGE ( 'NONE', *, *, #10671, .T. ) ;
#15463 = CARTESIAN_POINT ( 'NONE',  ( 6.999999999999992006, 2.775557561562891351E-14, 12.24999999999996980 ) ) ;
#15464 = CARTESIAN_POINT ( 'NONE',  ( 3.973110223767139626, -2.262956479381524922E-11, -3.565797985667441328 ) ) ;
#15465 = DIRECTION ( 'NONE',  ( -1.000000000000000000, -3.254448077276381206E-32, -1.066788928082016908E-26 ) ) ;
#15466 = CARTESIAN_POINT ( 'NONE',  ( -55.25320565519150051, 3.200000000000098765, 7.500000000000062172 ) ) ;
#15467 = CARTESIAN_POINT ( 'NONE',  ( 7.499999999999992895, -8.000000000000003553, 11.74999999999999645 ) ) ;
#15468 = EDGE_CURVE ( 'NONE', #273, #14077, #262, .T. ) ;
#15469 = CARTESIAN_POINT ( 'NONE',  ( -2.428612866367529932E-14, 60.00000000000000000, 6.938893903907228378E-15 ) ) ;
#15470 = DIRECTION ( 'NONE',  ( 0.000000000000000000, 0.000000000000000000, 1.000000000000000000 ) ) ;
#15471 = FACE_OUTER_BOUND ( 'NONE', #17126, .T. ) ;
#15472 = CONICAL_SURFACE ( 'NONE', #4194, 4.750000000000000888, 0.7853981633974430610 ) ;
#15473 = CARTESIAN_POINT ( 'NONE',  ( 2.918498775983380256E-10, 2.999999999003851503, -5.999999999999998224 ) ) ;
#15474 = DIRECTION ( 'NONE',  ( -2.220446049250313081E-16, 1.000000000000000000, -7.025792437124636392E-31 ) ) ;
#15475 = EDGE_LOOP ( 'NONE', ( #3365, #21081, #12807, #19162 ) ) ;
#15476 = CARTESIAN_POINT ( 'NONE',  ( 3.973110223767149840, -2.262799480050941678E-11, -3.565797985667468417 ) ) ;
#15477 = FACE_OUTER_BOUND ( 'NONE', #8759, .T. ) ;
#15478 = AXIS2_PLACEMENT_3D ( 'NONE', #14776, #787, #9833 ) ;
#15479 = ORIENTED_EDGE ( 'NONE', *, *, #6379, .F. ) ;
#15480 = EDGE_CURVE ( 'NONE', #1148, #12394, #12849, .T. ) ;
#15481 = AXIS2_PLACEMENT_3D ( 'NONE', #9780, #21625, #19499 ) ;
#15482 = ORIENTED_EDGE ( 'NONE', *, *, #22210, .T. ) ;
#15483 = ORIENTED_EDGE ( 'NONE', *, *, #2207, .F. ) ;
#15484 = PRODUCT_DEFINITION_SHAPE ( 'NONE', 'NONE',  #18401 ) ;
#15485 = EDGE_CURVE ( 'NONE', #16509, #1004, #9640, .T. ) ;
#15486 = ORIENTED_EDGE ( 'NONE', *, *, #14541, .T. ) ;
#15487 = DIRECTION ( 'NONE',  ( -0.9878135252003119593, 5.399917434947377318E-16, 0.1556420233463085001 ) ) ;
#15488 = DIRECTION ( 'NONE',  ( 1.000000000000000000, 2.168404344971017743E-16, -1.780660105995169760E-30 ) ) ;
#15489 = VERTEX_POINT ( 'NONE', #15056 ) ;
#15490 = CARTESIAN_POINT ( 'NONE',  ( 3.999999999999955147, -2.309401076758532678, -3.433295621305388678 ) ) ;
#15491 = PLANE ( 'NONE',  #1747 ) ;
#15492 = DIRECTION ( 'NONE',  ( -3.885780586188016830E-16, -4.437342591868156373E-31, 1.000000000000000000 ) ) ;
#15493 = DIRECTION ( 'NONE',  ( 3.885780586188016830E-16, 4.437342591868156373E-31, -1.000000000000000000 ) ) ;
#15494 = AXIS2_PLACEMENT_3D ( 'NONE', #15351, #21125, #11703 ) ;
#15495 = CARTESIAN_POINT ( 'NONE',  ( -10.49999999999998224, -13.50000000000003020, 5.750000000000032863 ) ) ;
#15496 = CARTESIAN_POINT ( 'NONE',  ( -7.748687480237880898, -0.2688970177183537813, 8.040801957829128099 ) ) ;
#15497 = CIRCLE ( 'NONE', #5743, 2.500000000000015543 ) ;
#15498 = AXIS2_PLACEMENT_3D ( 'NONE', #16503, #1924, #3810 ) ;
#15499 = ADVANCED_FACE ( 'NONE', ( #9776 ), #6022, .T. ) ;
#15500 = VECTOR ( 'NONE', #5869, 1000.000000000000000 ) ;
#15501 = DIRECTION ( 'NONE',  ( -1.387778780781450803E-15, 0.000000000000000000, 1.000000000000000000 ) ) ;
#15502 = DIRECTION ( 'NONE',  ( 0.000000000000000000, 4.190823558986606824E-31, -1.000000000000000000 ) ) ;
#15503 = CARTESIAN_POINT ( 'NONE',  ( 0.000000000000000000, -3.031088913245536087, -1.749999999999996447 ) ) ;
#15504 = CARTESIAN_POINT ( 'NONE',  ( 3.973110223765516036, -0.6902454861566473809, 3.565797985667351622 ) ) ;
#15505 = CARTESIAN_POINT ( 'NONE',  ( -5.197224361976157780, 35.99999999900384751, -25.50000000000000000 ) ) ;
#15506 = CARTESIAN_POINT ( 'NONE',  ( 42.50000000000014921, 2.499999999999998668, -12.49999999999998401 ) ) ;
#15507 = VECTOR ( 'NONE', #5479, 1000.000000000000000 ) ;
#15508 = CIRCLE ( 'NONE', #16679, 0.5000000000000001110 ) ;
#15509 = CIRCLE ( 'NONE', #16628, 4.582731094065982447 ) ;
#15510 = EDGE_LOOP ( 'NONE', ( #9455, #9832, #6210, #19078 ) ) ;
#15511 = AXIS2_PLACEMENT_3D ( 'NONE', #20425, #13596, #2882 ) ;
#15512 = CIRCLE ( 'NONE', #18169, 0.8000000000000090372 ) ;
#15513 = AXIS2_PLACEMENT_3D ( 'NONE', #8727, #10939, #14020 ) ;
#15515 = VERTEX_POINT ( 'NONE', #15180 ) ;
#15514 = VERTEX_POINT ( 'NONE', #11528 ) ;
#15516 = CARTESIAN_POINT ( 'NONE',  ( -65.47859922179033276, 4.857225732735059864E-14, -11.38422848940298593 ) ) ;
#15517 = CYLINDRICAL_SURFACE ( 'NONE', #10339, 0.5000000000000004441 ) ;
#15518 = DIRECTION ( 'NONE',  ( -0.6819983600625055820, -0.7313537016191637985, -4.996142016973858765E-16 ) ) ;
#15519 = ORIENTED_EDGE ( 'NONE', *, *, #16690, .T. ) ;
#15520 = DIRECTION ( 'NONE',  ( -1.733449886265891589E-32, 4.190823558986610327E-31, -1.000000000000000000 ) ) ;
#15521 = CARTESIAN_POINT ( 'NONE',  ( 4.113620667976089607, -1.750000000000025757, 2.374999999999986677 ) ) ;
#15522 = CARTESIAN_POINT ( 'NONE',  ( 57.70499590015723612, 1.828384254047854540, 6.000000000000136779 ) ) ;
#15523 = DIRECTION ( 'NONE',  ( 0.000000000000000000, -1.000000000000000000, 0.000000000000000000 ) ) ;
#15524 = ADVANCED_FACE ( 'NONE', ( #16813 ), #13314, .T. ) ;
#15525 = CYLINDRICAL_SURFACE ( 'NONE', #8825, 4.750000000000000000 ) ;
#15526 = VECTOR ( 'NONE', #17144, 1000.000000000000000 ) ;
#15527 = AXIS2_PLACEMENT_3D ( 'NONE', #19355, #10296, #9756 ) ;
#15528 = DIRECTION ( 'NONE',  ( 0.000000000000000000, 1.000000000000000000, 0.000000000000000000 ) ) ;
#15529 = AXIS2_PLACEMENT_3D ( 'NONE', #1755, #16207, #7301 ) ;
#15530 = FACE_OUTER_BOUND ( 'NONE', #16515, .T. ) ;
#15531 = CIRCLE ( 'NONE', #6531, 7.000000000000075495 ) ;
#15532 = LINE ( 'NONE', #1765, #12667 ) ;
#15533 = CIRCLE ( 'NONE', #5412, 0.4999999999999995559 ) ;
#15534 = VECTOR ( 'NONE', #17661, 1000.000000000000000 ) ;
#15535 = EDGE_CURVE ( 'NONE', #18914, #2832, #8718, .T. ) ;
#15536 = DIRECTION ( 'NONE',  ( -1.000000000000000000, 4.615739097524200579E-16, 1.134196829589820086E-15 ) ) ;
#15537 = CARTESIAN_POINT ( 'NONE',  ( -42.54314575050793934, -4.800000000000019362, 7.500000000000062172 ) ) ;
#15538 = ADVANCED_FACE ( 'NONE', ( #966 ), #2708, .T. ) ;
#15539 = ORIENTED_EDGE ( 'NONE', *, *, #12707, .T. ) ;
#15541 = ORIENTED_EDGE ( 'NONE', *, *, #11402, .F. ) ;
#15540 = ORIENTED_EDGE ( 'NONE', *, *, #10420, .F. ) ;
#15542 = ORIENTED_EDGE ( 'NONE', *, *, #11348, .F. ) ;
#15543 = AXIS2_PLACEMENT_3D ( 'NONE', #193, #11424, #22135 ) ;
#15545 = ORIENTED_EDGE ( 'NONE', *, *, #2109, .T. ) ;
#15544 = ORIENTED_EDGE ( 'NONE', *, *, #20753, .T. ) ;
#15546 = CIRCLE ( 'NONE', #6917, 0.4999999999999993894 ) ;
#15547 = EDGE_LOOP ( 'NONE', ( #2462, #12886, #3549, #23186 ) ) ;
#15548 = FACE_OUTER_BOUND ( 'NONE', #4248, .T. ) ;
#15549 = AXIS2_PLACEMENT_3D ( 'NONE', #19815, #12751, #9457 ) ;
#15550 = CARTESIAN_POINT ( 'NONE',  ( 0.3126073911696447549, 2.020725942163688504, 3.499999999999997780 ) ) ;
#15551 = EDGE_CURVE ( 'NONE', #4929, #4634, #20757, .T. ) ;
#15552 = ADVANCED_FACE ( 'NONE', ( #6481 ), #5725, .T. ) ;
#15553 = FACE_OUTER_BOUND ( 'NONE', #14764, .T. ) ;
#15554 = CYLINDRICAL_SURFACE ( 'NONE', #22192, 6.000000000000047073 ) ;
#15555 = CARTESIAN_POINT ( 'NONE',  ( -8.216162181246556173, -1.557177370613358702, 7.299847320220810509 ) ) ;
#15556 = EDGE_CURVE ( 'NONE', #14484, #20416, #13543, .T. ) ;
#15557 = CARTESIAN_POINT ( 'NONE',  ( -2.742413778650712342, 1.749999999999973799, 4.749999999999999112 ) ) ;
#15558 = CYLINDRICAL_SURFACE ( 'NONE', #7647, 2.550000000000010481 ) ;
#15559 = CARTESIAN_POINT ( 'NONE',  ( -52.60445557845689990, 2.700000000000056577, 15.85914177512520773 ) ) ;
#15560 = CARTESIAN_POINT ( 'NONE',  ( -6.000000000000088818, -8.000000000000042633, 8.000000000000062172 ) ) ;
#15561 = CARTESIAN_POINT ( 'NONE',  ( 0.000000000000000000, 0.000000000000000000, -4.484454397937119197 ) ) ;
#15562 = AXIS2_PLACEMENT_3D ( 'NONE', #7783, #7362, #734 ) ;
#15563 = ADVANCED_FACE ( 'NONE', ( #9897 ), #6374, .T. ) ;
#15564 = CLOSED_SHELL ( 'NONE', ( #20479, #7511, #15848, #15688, #9078, #7939, #16722, #18792, #22107, #6765, #7089, #18429, #21616, #9708, #3356, #19875, #15226, #15743, #4810, #8819, #15087, #5963, #9977 ) ) ;
#15565 = FACE_OUTER_BOUND ( 'NONE', #14487, .T. ) ;
#15566 = EDGE_CURVE ( 'NONE', #10116, #145, #8781, .T. ) ;
#15567 = CARTESIAN_POINT ( 'NONE',  ( -3.999999999999735323, 0.8576368993457454959, -3.433240632782417645 ) ) ;
#15568 = CARTESIAN_POINT ( 'NONE',  ( 3.972066048304754737, -2.740530939476236050, 2.384802634787871689 ) ) ;
#15569 = AXIS2_PLACEMENT_3D ( 'NONE', #20284, #20392, #6276 ) ;
#15570 = EDGE_CURVE ( 'NONE', #19569, #21118, #22607, .T. ) ;
#15571 = ORIENTED_EDGE ( 'NONE', *, *, #1818, .T. ) ;
#15573 = EDGE_LOOP ( 'NONE', ( #19976, #7131, #9277, #9365 ) ) ;
#15572 = ORIENTED_EDGE ( 'NONE', *, *, #9406, .T. ) ;
#15574 = SHAPE_REPRESENTATION ( 'Half Handle', ( #22115 ), #712 ) ;
#15575 = ORIENTED_EDGE ( 'NONE', *, *, #14541, .F. ) ;
#15576 = VERTEX_POINT ( 'NONE', #20724 ) ;
#15577 = ADVANCED_FACE ( 'NONE', ( #4587 ), #11767, .T. ) ;
#15578 = VERTEX_POINT ( 'NONE', #5752 ) ;
#15579 = DIRECTION ( 'NONE',  ( -0.000000000000000000, -0.000000000000000000, 1.000000000000000000 ) ) ;
#15580 = EDGE_CURVE ( 'NONE', #6911, #20801, #16543, .T. ) ;
#15581 = FACE_BOUND ( 'NONE', #16836, .T. ) ;
#15582 = ORIENTED_EDGE ( 'NONE', *, *, #5054, .F. ) ;
#15583 = CARTESIAN_POINT ( 'NONE',  ( -5.742213840172610633E-15, -12.15667283655309205, -12.14055452724117679 ) ) ;
#15584 = CARTESIAN_POINT ( 'NONE',  ( -61.45000000000044338, -7.672331518739547608E-14, -2.000000000000002220 ) ) ;
#15585 = CARTESIAN_POINT ( 'NONE',  ( -95.70000000000062812, -0.5000000000000975886, 8.000000000000062172 ) ) ;
#15586 = CARTESIAN_POINT ( 'NONE',  ( -3.999999999708139686, 13.32455531934060744, -29.00000000000000355 ) ) ;
#15587 = CARTESIAN_POINT ( 'NONE',  ( -6.000000000000074607, 1.999999999999960032, 7.500000000000062172 ) ) ;
#15588 = EDGE_CURVE ( 'NONE', #16689, #12862, #11698, .T. ) ;
#15589 = CARTESIAN_POINT ( 'NONE',  ( 1.199999999999992628, 1.384721729257273387E-16, 4.582731094065980670 ) ) ;
#15590 = CARTESIAN_POINT ( 'NONE',  ( -50.65685424949273141, 7.200000000000025935, 8.000000000000076383 ) ) ;
#15591 = CARTESIAN_POINT ( 'NONE',  ( 4.000000000000003553, 2.309401076758480720, -5.600000000000000533 ) ) ;
#15592 = EDGE_CURVE ( 'NONE', #18277, #14827, #694, .T. ) ;
#15593 = PLANE ( 'NONE',  #6156 ) ;
#15594 = CARTESIAN_POINT ( 'NONE',  ( 0.000000000000000000, 1.750000000000001554, 0.000000000000000000 ) ) ;
#15595 = ORIENTED_EDGE ( 'NONE', *, *, #8990, .F. ) ;
#15596 = CIRCLE ( 'NONE', #9595, 4.749999999999986677 ) ;
#15597 =( LENGTH_UNIT ( ) NAMED_UNIT ( * ) SI_UNIT ( .MILLI., .METRE. ) );
#15598 = DIRECTION ( 'NONE',  ( 0.000000000000000000, 0.000000000000000000, 1.000000000000000000 ) ) ;
#15599 = AXIS2_PLACEMENT_3D ( 'NONE', #20357, #11636, #8121 ) ;
#15600 = DIRECTION ( 'NONE',  ( 0.7071067811865474617, -0.7071067811865474617, 0.000000000000000000 ) ) ;
#15601 = ORIENTED_EDGE ( 'NONE', *, *, #4648, .T. ) ;
#15602 = EDGE_LOOP ( 'NONE', ( #18913, #20488, #9369, #20559 ) ) ;
#15603 = ORIENTED_EDGE ( 'NONE', *, *, #18305, .T. ) ;
#15604 = ORIENTED_EDGE ( 'NONE', *, *, #5341, .F. ) ;
#15605 = CARTESIAN_POINT ( 'NONE',  ( -3.999999999708153453, 42.99999999900385461, -29.00000000000000355 ) ) ;
#15606 = SPHERICAL_SURFACE ( 'NONE', #14797, 0.5000000000000000000 ) ;
#15607 = ORIENTED_EDGE ( 'NONE', *, *, #4874, .F. ) ;
#15608 = AXIS2_PLACEMENT_3D ( 'NONE', #11132, #9261, #14546 ) ;
#15609 = CARTESIAN_POINT ( 'NONE',  ( 2.298974087845766956, 1.453757124411862778, 4.749999999999999112 ) ) ;
#15610 = CARTESIAN_POINT ( 'NONE',  ( 2.775557561562891351E-14, 10.49999999999999822, -6.499999999999950262 ) ) ;
#15611 = CARTESIAN_POINT ( 'NONE',  ( 0.000000000000000000, -3.031088913245480576, 1.749999999999994671 ) ) ;
#15612 = CARTESIAN_POINT ( 'NONE',  ( -4.550510256924974684, 35.99999999900384751, -19.50000000000000355 ) ) ;
#15613 = DIRECTION ( 'NONE',  ( -1.000000000000000000, -2.699383410053119644E-30, -3.330669073875432643E-16 ) ) ;
#15614 = CARTESIAN_POINT ( 'NONE',  ( -7.856071383949472242, -0.04768060911160423160, 7.015054140272269478 ) ) ;
#15615 = EDGE_CURVE ( 'NONE', #22415, #16051, #10581, .T. ) ;
#15616 = DIRECTION ( 'NONE',  ( 4.190823558986625216E-31, -1.000000000000000000, 4.190823558986625216E-31 ) ) ;
#15617 = DIRECTION ( 'NONE',  ( -0.000000000000000000, 1.000000000000000000, -0.000000000000000000 ) ) ;
#15618 = ORIENTED_EDGE ( 'NONE', *, *, #3895, .F. ) ;
#15619 = CARTESIAN_POINT ( 'NONE',  ( 30.00000000029184832, -9.961476088449217059E-10, -5.999999999999998224 ) ) ;
#15620 = DIRECTION ( 'NONE',  ( -0.7071067811865492381, -0.7071067811865457964, 0.000000000000000000 ) ) ;
#15621 = DIRECTION ( 'NONE',  ( -2.220446049250313081E-16, 1.000000000000000000, -7.025792437124636392E-31 ) ) ;
#15622 = EDGE_CURVE ( 'NONE', #7652, #8024, #4932, .T. ) ;
#15623 = PRESENTATION_LAYER_ASSIGNMENT (  '', '', ( #1366 ) ) ;
#15624 = DIRECTION ( 'NONE',  ( 1.454462294001240516E-30, 1.000000000000000000, 0.000000000000000000 ) ) ;
#15625 = ORIENTED_EDGE ( 'NONE', *, *, #13585, .F. ) ;
#15626 = EDGE_CURVE ( 'NONE', #17223, #2802, #22237, .T. ) ;
#15627 = TOROIDAL_SURFACE ( 'NONE', #4734, 4.500000000000000888, 0.5000000000000000000 ) ;
#15628 = ORIENTED_EDGE ( 'NONE', *, *, #5918, .T. ) ;
#15629 = DIRECTION ( 'NONE',  ( -7.860214984770699307E-18, 1.409037165336591006E-16, 1.000000000000000000 ) ) ;
#15631 = ORIENTED_EDGE ( 'NONE', *, *, #19750, .T. ) ;
#15630 = EDGE_LOOP ( 'NONE', ( #4522, #10254, #14997, #5822 ) ) ;
#15632 = CARTESIAN_POINT ( 'NONE',  ( 0.000000000000000000, 0.000000000000000000, 0.000000000000000000 ) ) ;
#15633 = LINE ( 'NONE', #6709, #8843 ) ;
#15634 = CIRCLE ( 'NONE', #20914, 0.5000000000000000000 ) ;
#15635 = DIRECTION ( 'NONE',  ( -1.000000000000000000, 0.000000000000000000, 0.000000000000000000 ) ) ;
#15636 = VERTEX_POINT ( 'NONE', #18563 ) ;
#15637 = ADVANCED_BREP_SHAPE_REPRESENTATION ( '', ( #5189, #22115 ), #4465 ) ;
#15638 = DIRECTION ( 'NONE',  ( -0.7071067811865485719, 0.7071067811865464625, 1.010793663541191485E-16 ) ) ;
#15639 = DIRECTION ( 'NONE',  ( 3.032184104443272185E-30, 1.000000000000000000, -7.395570986447005381E-32 ) ) ;
#15640 = FACE_OUTER_BOUND ( 'NONE', #14043, .T. ) ;
#15641 = FACE_OUTER_BOUND ( 'NONE', #17041, .T. ) ;
#15642 = DIRECTION ( 'NONE',  ( 8.438582421954109416E-32, 0.000000000000000000, 1.000000000000000000 ) ) ;
#15643 = DIRECTION ( 'NONE',  ( -3.885780586188016830E-16, -4.437342591868156373E-31, 1.000000000000000000 ) ) ;
#15644 = DIRECTION ( 'NONE',  ( -1.000000000000000000, 1.276756478318923119E-15, -1.333893503340766797E-15 ) ) ;
#15645 = DIRECTION ( 'NONE',  ( -1.000000000000000000, 0.000000000000000000, 0.000000000000000000 ) ) ;
#15646 = CARTESIAN_POINT ( 'NONE',  ( 4.082498951862915781, -4.041451884327383226, -6.134919877127760970E-18 ) ) ;
#15647 = ORIENTED_EDGE ( 'NONE', *, *, #15709, .T. ) ;
#15648 = CARTESIAN_POINT ( 'NONE',  ( -68.59459193786533149, 38.58681605307295115, 46.76570243528393434 ) ) ;
#15650 = ORIENTED_EDGE ( 'NONE', *, *, #811, .F. ) ;
#15649 = EDGE_LOOP ( 'NONE', ( #8086, #22845 ) ) ;
#15651 = ADVANCED_FACE ( 'NONE', ( #10908 ), #5333, .T. ) ;
#15652 = ORIENTED_EDGE ( 'NONE', *, *, #15832, .F. ) ;
#15654 = EDGE_LOOP ( 'NONE', ( #6697, #14423, #6673, #10087 ) ) ;
#15653 = VERTEX_POINT ( 'NONE', #14799 ) ;
#15655 = VERTEX_POINT ( 'NONE', #7860 ) ;
#15656 = FACE_OUTER_BOUND ( 'NONE', #11237, .T. ) ;
#15657 = CARTESIAN_POINT ( 'NONE',  ( 0.000000000000000000, 0.000000000000000000, 0.000000000000000000 ) ) ;
#15658 = CARTESIAN_POINT ( 'NONE',  ( 2.918498775983380256E-10, -9.961476088449217059E-10, -19.00000000000000355 ) ) ;
#15659 = LINE ( 'NONE', #8732, #14165 ) ;
#15660 = CARTESIAN_POINT ( 'NONE',  ( -7.168696526429558347, -0.3737769141893427793, 8.340670630249109152 ) ) ;
#15661 = DIRECTION ( 'NONE',  ( -2.013525853228507892E-32, -6.902532920683810383E-31, 1.000000000000000000 ) ) ;
#15662 = AXIS2_PLACEMENT_3D ( 'NONE', #6782, #23146, #19597 ) ;
#15663 = DIRECTION ( 'NONE',  ( 3.885780586188016830E-16, 4.437342591868156373E-31, -1.000000000000000000 ) ) ;
#15664 = AXIS2_PLACEMENT_3D ( 'NONE', #3545, #1661, #1874 ) ;
#15665 = DIRECTION ( 'NONE',  ( -0.4472135954999586493, 0.7745966692414837373, -0.4472135954999567065 ) ) ;
#15666 = CARTESIAN_POINT ( 'NONE',  ( 4.052432342741398408, 1.393590342654249525, 3.567979436357390011 ) ) ;
#15667 = DIRECTION ( 'NONE',  ( -0.000000000000000000, -0.000000000000000000, 1.000000000000000000 ) ) ;
#15668 = PLANE ( 'NONE',  #4383 ) ;
#15669 = CIRCLE ( 'NONE', #9303, 4.000000000000000000 ) ;
#15670 = DIRECTION ( 'NONE',  ( 2.220446049250313081E-16, -1.000000000000000000, 7.025792437124636392E-31 ) ) ;
#15671 = DIRECTION ( 'NONE',  ( -0.8191520442889927978, 0.000000000000000000, -0.5735764363510447161 ) ) ;
#15672 = DIRECTION ( 'NONE',  ( 1.000000000000000000, 2.172745813409351317E-17, 9.470910429910635790E-17 ) ) ;
#15673 = PRODUCT_DEFINITION_SHAPE ( 'NONE', 'NONE',  #23271 ) ;
#15674 = AXIS2_PLACEMENT_3D ( 'NONE', #3814, #10987, #18185 ) ;
#15675 = ORIENTED_EDGE ( 'NONE', *, *, #4798, .T. ) ;
#15676 = ADVANCED_FACE ( 'NONE', ( #20220 ), #7513, .T. ) ;
#15678 = ORIENTED_EDGE ( 'NONE', *, *, #393, .T. ) ;
#15677 = ORIENTED_EDGE ( 'NONE', *, *, #7242, .T. ) ;
#15679 = VECTOR ( 'NONE', #21690, 1000.000000000000000 ) ;
#15680 = ADVANCED_FACE ( 'NONE', ( #21757 ), #4089, .T. ) ;
#15681 = ORIENTED_EDGE ( 'NONE', *, *, #15480, .F. ) ;
#15682 = VERTEX_POINT ( 'NONE', #18333 ) ;
#15683 = CIRCLE ( 'NONE', #10430, 4.750000000000000000 ) ;
#15684 = ORIENTED_EDGE ( 'NONE', *, *, #22469, .T. ) ;
#15685 = ORIENTED_EDGE ( 'NONE', *, *, #9053, .T. ) ;
#15686 = DIRECTION ( 'NONE',  ( 1.000000000000000000, 0.000000000000000000, 0.000000000000000000 ) ) ;
#15687 = EDGE_CURVE ( 'NONE', #7125, #5612, #11266, .T. ) ;
#15688 = ADVANCED_FACE ( 'NONE', ( #18222 ), #18443, .F. ) ;
#15689 = CARTESIAN_POINT ( 'NONE',  ( -4.000000000000058620, -2.309401076758546445, -3.433295621305388678 ) ) ;
#15690 = ORIENTED_EDGE ( 'NONE', *, *, #21187, .T. ) ;
#15691 = DIRECTION ( 'NONE',  ( -0.000000000000000000, -0.000000000000000000, 1.000000000000000000 ) ) ;
#15692 = EDGE_CURVE ( 'NONE', #902, #6061, #10763, .T. ) ;
#15693 = CARTESIAN_POINT ( 'NONE',  ( 4.050480423730732582, 1.376911654797405848, -3.567926555162023394 ) ) ;
#15694 = CARTESIAN_POINT ( 'NONE',  ( 24.75000000000000355, 2.000000000000029310, -0.2500000000000002220 ) ) ;
#15695 = DIRECTION ( 'NONE',  ( -1.000000000000000000, -4.440892098500626162E-16, 5.551115123125782702E-16 ) ) ;
#15696 = CARTESIAN_POINT ( 'NONE',  ( -8.137537312224724317, -0.5625089224579539193, 7.396067884835295203 ) ) ;
#15697 = CARTESIAN_POINT ( 'NONE',  ( 5.036205380386659769, -1.584759246591014747, 0.7770364038185700872 ) ) ;
#15698 = DIRECTION ( 'NONE',  ( 3.070652698126927723E-17, 1.000000000000000000, -4.167305704548413124E-17 ) ) ;
#15699 = COLOUR_RGB ( '', 0.40784314, 0.44705882, 0.49803922) ;
#15700 = FACE_OUTER_BOUND ( 'NONE', #19724, .T. ) ;
#15701 = FACE_BOUND ( 'NONE', #18621, .T. ) ;
#15702 = CARTESIAN_POINT ( 'NONE',  ( -6.899936419963482059, 13.99939863585067990, -18.20594370724277056 ) ) ;
#15703 = CIRCLE ( 'NONE', #9320, 4.000000000000000000 ) ;
#15704 = DIRECTION ( 'NONE',  ( 0.000000000000000000, 1.000000000000000000, 0.000000000000000000 ) ) ;
#15705 = ADVANCED_FACE ( 'NONE', ( #2088 ), #22214, .T. ) ;
#15706 = ORIENTED_EDGE ( 'NONE', *, *, #55, .F. ) ;
#15707 = ADVANCED_FACE ( 'NONE', ( #1971 ), #18096, .T. ) ;
#15708 = AXIS2_PLACEMENT_3D ( 'NONE', #1766, #19890, #3758 ) ;
#15709 = EDGE_CURVE ( 'NONE', #11317, #20537, #12478, .T. ) ;
#15710 = DIRECTION ( 'NONE',  ( -1.000000000000000000, -2.699383410053119644E-30, -3.330669073875432643E-16 ) ) ;
#15711 = CIRCLE ( 'NONE', #22865, 3.999999999999999112 ) ;
#15712 = DIRECTION ( 'NONE',  ( -0.7313537016191730133, 0.6819983600624958120, -5.924440990721418971E-17 ) ) ;
#15713 = VECTOR ( 'NONE', #4153, 1000.000000000000000 ) ;
#15715 = ORIENTED_EDGE ( 'NONE', *, *, #22752, .T. ) ;
#15714 = ORIENTED_EDGE ( 'NONE', *, *, #4422, .F. ) ;
#15716 = B_SPLINE_CURVE_WITH_KNOTS ( 'NONE', 3,
 ( #5535, #19990, #706, #18111, #1986, #9176, #18577, #14688, #3982, #14581, #9632, #4206, #20236, #3865 ),
 .UNSPECIFIED., .F., .F.,
 ( 4, 2, 2, 2, 2, 2, 4 ),
 ( 0.000000000000000000, 0.001011182963765811091, 0.001516774445648716094, 0.002022365927531621314, 0.002527957409414526100, 0.003033548891297431320, 0.004044731855063247832 ),
 .UNSPECIFIED. ) ;
#15717 = ORIENTED_EDGE ( 'NONE', *, *, #11582, .F. ) ;
#15718 = EDGE_CURVE ( 'NONE', #14225, #21501, #16941, .T. ) ;
#15719 = ORIENTED_EDGE ( 'NONE', *, *, #5799, .T. ) ;
#15720 = STYLED_ITEM ( 'NONE', ( #21720 ), #7243 ) ;
#15721 = CARTESIAN_POINT ( 'NONE',  ( -12.85000000000001386, -1.999999999999998224, -6.249999999999992006 ) ) ;
#15722 = LINE ( 'NONE', #15949, #12527 ) ;
#15723 = ADVANCED_FACE ( 'NONE', ( #6984 ), #19322, .F. ) ;
#15724 = DIRECTION ( 'NONE',  ( -2.013525853228507892E-32, -6.902532920683810383E-31, 1.000000000000000000 ) ) ;
#15725 = CARTESIAN_POINT ( 'NONE',  ( 4.055492966679613787, 3.795017426214645884, -0.5629142681441038354 ) ) ;
#15726 = ADVANCED_FACE ( 'NONE', ( #12367 ), #21331, .F. ) ;
#15727 = CARTESIAN_POINT ( 'NONE',  ( 119.5756419024615553, -11.00000000000006573, 6.500000000000012434 ) ) ;
#15728 = AXIS2_PLACEMENT_3D ( 'NONE', #1174, #948, #22465 ) ;
#15729 = VECTOR ( 'NONE', #8196, 1000.000000000000000 ) ;
#15730 = CARTESIAN_POINT ( 'NONE',  ( 12.84999999999997300, -12.00000000000008704, -2.549999999999958966 ) ) ;
#15731 = DIRECTION ( 'NONE',  ( 1.000000000000000000, 2.699383410053118943E-30, 2.668805347656595124E-16 ) ) ;
#15732 = FACE_OUTER_BOUND ( 'NONE', #19244, .T. ) ;
#15733 = LINE ( 'NONE', #3621, #16708 ) ;
#15734 = DIRECTION ( 'NONE',  ( -1.756300210255732376E-61, 4.190823558986625216E-31, 1.000000000000000000 ) ) ;
#15735 = DIRECTION ( 'NONE',  ( 7.860214984770699307E-18, -1.409037165336591006E-16, -1.000000000000000000 ) ) ;
#15736 = DIRECTION ( 'NONE',  ( 3.885780586188016830E-16, 4.437342591868156373E-31, -1.000000000000000000 ) ) ;
#15737 = CARTESIAN_POINT ( 'NONE',  ( -0.5276280594138318403, 4.314175951382505758, -3.320322319201708616 ) ) ;
#15738 = DIRECTION ( 'NONE',  ( 0.000000000000000000, -7.888609052210128564E-31, 1.000000000000000000 ) ) ;
#15739 = VERTEX_POINT ( 'NONE', #16548 ) ;
#15740 = AXIS2_PLACEMENT_3D ( 'NONE', #18296, #21833, #11110 ) ;
#15741 = CIRCLE ( 'NONE', #4477, 2.500000000000003997 ) ;
#15742 = ORIENTED_EDGE ( 'NONE', *, *, #14102, .F. ) ;
#15743 = ADVANCED_FACE ( 'NONE', ( #19672 ), #9829, .T. ) ;
#15744 = DIRECTION ( 'NONE',  ( 1.000000000000000000, 3.254448077276381206E-32, 1.066788928082016908E-26 ) ) ;
#15746 = EDGE_LOOP ( 'NONE', ( #1351, #16054, #11817, #15462 ) ) ;
#15745 = ORIENTED_EDGE ( 'NONE', *, *, #7294, .F. ) ;
#15747 = EDGE_CURVE ( 'NONE', #19664, #14175, #1439, .T. ) ;
#15748 = VECTOR ( 'NONE', #2949, 1000.000000000000000 ) ;
#15749 = CARTESIAN_POINT ( 'NONE',  ( -0.1750025118122067458, -4.719839900820679723, -3.469254087858268054 ) ) ;
#15750 = ORIENTED_EDGE ( 'NONE', *, *, #12975, .F. ) ;
#15751 = FACE_OUTER_BOUND ( 'NONE', #19783, .T. ) ;
#15752 = EDGE_CURVE ( 'NONE', #15826, #22801, #91, .T. ) ;
#15753 = MECHANICAL_DESIGN_GEOMETRIC_PRESENTATION_REPRESENTATION (  '', ( #9018 ), #7153 ) ;
#15754 = DIRECTION ( 'NONE',  ( 0.000000000000000000, 0.000000000000000000, -1.000000000000000000 ) ) ;
#15755 = EDGE_LOOP ( 'NONE', ( #15790, #6103, #16725, #5912 ) ) ;
#15756 = DIRECTION ( 'NONE',  ( -2.220446049250313081E-16, 1.000000000000000000, -7.025792437124636392E-31 ) ) ;
#15757 = DIRECTION ( 'NONE',  ( 8.438582421954109416E-32, 0.000000000000000000, 1.000000000000000000 ) ) ;
#15758 = LINE ( 'NONE', #23075, #21072 ) ;
#15759 = DIRECTION ( 'NONE',  ( -0.7071067811865475727, -0.7071067811865475727, 0.000000000000000000 ) ) ;
#15760 = DIRECTION ( 'NONE',  ( -0.5000000000000001110, 0.000000000000000000, -0.8660254037844385966 ) ) ;
#15761 = FACE_OUTER_BOUND ( 'NONE', #13944, .T. ) ;
#15762 = DIRECTION ( 'NONE',  ( 1.000000000000000000, -4.440892098500651800E-16, -7.860214984771115307E-18 ) ) ;
#15763 = DIRECTION ( 'NONE',  ( 1.000000000000000000, 2.220446049250314067E-16, -5.825996348268307008E-33 ) ) ;
#15764 = AXIS2_PLACEMENT_3D ( 'NONE', #20398, #6399, #7922 ) ;
#15765 = PRODUCT_DEFINITION_FORMATION_WITH_SPECIFIED_SOURCE ( 'ANY', '', #2909, .NOT_KNOWN. ) ;
#15766 = EDGE_LOOP ( 'NONE', ( #1937, #11891, #1295, #12984 ) ) ;
#15767 = CARTESIAN_POINT ( 'NONE',  ( -92.38743622395921307, 28.87133558231438712, 24.16570243528395068 ) ) ;
#15769 = ORIENTED_EDGE ( 'NONE', *, *, #3475, .T. ) ;
#15768 = VERTEX_POINT ( 'NONE', #3859 ) ;
#15770 = ORIENTED_EDGE ( 'NONE', *, *, #6940, .F. ) ;
#15772 = VERTEX_POINT ( 'NONE', #10373 ) ;
#15771 = ORIENTED_EDGE ( 'NONE', *, *, #15275, .T. ) ;
#15773 = DIRECTION ( 'NONE',  ( -1.000000000000000000, 1.276756478318923119E-15, -1.239088197126283964E-15 ) ) ;
#15774 = CARTESIAN_POINT ( 'NONE',  ( 108.2426266706971205, -10.52760560296367487, -6.500000000000075495 ) ) ;
#15775 = SURFACE_SIDE_STYLE ('',( #10601 ) ) ;
#15776 = CARTESIAN_POINT ( 'NONE',  ( 0.000000000000000000, -14.99999999999997513, -1.387778780781445676E-14 ) ) ;
#15777 = AXIS2_PLACEMENT_3D ( 'NONE', #6048, #1111, #11443 ) ;
#15778 = DIRECTION ( 'NONE',  ( -3.241725282392603095E-30, -1.000000000000000000, 2.218671295934100958E-31 ) ) ;
#15779 = DIRECTION ( 'NONE',  ( -1.000000000000000000, -1.700709290173333260E-16, 0.000000000000000000 ) ) ;
#15780 = CARTESIAN_POINT ( 'NONE',  ( -6.938893903907228378E-14, 4.999999999999976907, -4.163336342344337027E-14 ) ) ;
#15781 = DIRECTION ( 'NONE',  ( 7.860214984771176937E-18, 1.409037165336591006E-16, 1.000000000000000000 ) ) ;
#15782 = CARTESIAN_POINT ( 'NONE',  ( -12.85000000000001386, -12.00000000000006928, 4.163336342344337027E-14 ) ) ;
#15783 = CARTESIAN_POINT ( 'NONE',  ( 3.950250160040162051, -0.7258013381035534062, 3.499999999999996003 ) ) ;
#15784 = LINE ( 'NONE', #11802, #4586 ) ;
#15785 = EDGE_CURVE ( 'NONE', #3212, #477, #3439, .T. ) ;
#15786 = CARTESIAN_POINT ( 'NONE',  ( -50.65685424949274562, -1.040834085586084257E-13, 8.000000000000062172 ) ) ;
#15787 = CARTESIAN_POINT ( 'NONE',  ( -7.500000000000005329, -11.56013155386942692, 9.052558787159771470 ) ) ;
#15788 = CARTESIAN_POINT ( 'NONE',  ( -4.197312064133520870, -0.8182229787991075476, -3.502518405183900008 ) ) ;
#15789 = CARTESIAN_POINT ( 'NONE',  ( -50.65685424949280247, -1.040834085586084257E-13, 7.500000000000062172 ) ) ;
#15790 = ORIENTED_EDGE ( 'NONE', *, *, #15901, .T. ) ;
#15791 = VECTOR ( 'NONE', #126, 1000.000000000000000 ) ;
#15793 = ORIENTED_EDGE ( 'NONE', *, *, #5833, .F. ) ;
#15792 = ORIENTED_EDGE ( 'NONE', *, *, #12818, .F. ) ;
#15794 = ORIENTED_EDGE ( 'NONE', *, *, #4802, .T. ) ;
#15795 =( BOUNDED_SURFACE ( )  B_SPLINE_SURFACE ( 3, 2, ( 
 ( #20404, #11566, #6962 ),
 ( #16852, #15083, #22515 ),
 ( #22280, #10155, #11448 ),
 ( #6404, #17204, #8044 ),
 ( #13573, #6174, #18750 ),
 ( #20756, #10041, #2633 ),
 ( #22627, #6286, #9808 ),
 ( #16961, #15206, #8283 ),
 ( #22398, #4510, #15439 ),
 ( #6516, #13691, #4740 ),
 ( #14121, #14242, #16450 ),
 ( #19770, #10818, #21 ),
 ( #8833, #3541, #21433 ),
 ( #129, #10919, #1762 ) ),
 .UNSPECIFIED., .F., .F., .T. ) 
 B_SPLINE_SURFACE_WITH_KNOTS ( ( 4, 2, 2, 2, 2, 2, 4 ),
 ( 3, 3 ),
 ( 2.168404344971008868E-19, 0.0009656398008937972606, 0.001448459701340695837, 0.001931279601787594304, 0.002414099502234492989, 0.002896919402681391240, 0.003862559203575188175 ),
 ( 0.000000000000000000, 1.000000000000000000 ),
 .UNSPECIFIED. ) 
 GEOMETRIC_REPRESENTATION_ITEM ( )  RATIONAL_B_SPLINE_SURFACE ( (
 ( 1.000000000000000000, 0.7071067811865452413, 1.000000000000000000),
 ( 1.000000000000000000, 0.6907538105666497508, 1.000000000000000000),
 ( 1.000000000000000000, 0.6765417438350778134, 1.000000000000000000),
 ( 1.000000000000000000, 0.6623232117677899655, 1.000000000000000000),
 ( 1.000000000000000000, 0.6588386061806286165, 1.000000000000000000),
 ( 1.000000000000000000, 0.6547992448371706686, 1.000000000000000000),
 ( 1.000000000000000000, 0.6542040191407613170, 1.000000000000000000),
 ( 1.000000000000000000, 0.6557724471763412000, 1.000000000000000000),
 ( 1.000000000000000000, 0.6579729115736956402, 1.000000000000000000),
 ( 1.000000000000000000, 0.6644691908065332164, 1.000000000000000000),
 ( 1.000000000000000000, 0.6687559023949577464, 1.000000000000000000),
 ( 1.000000000000000000, 0.6835702420293556791, 1.000000000000000000),
 ( 1.000000000000000000, 0.6960226107070669466, 1.000000000000000000),
 ( 1.000000000000000000, 0.7071067811865451302, 1.000000000000000000) ) ) 
 REPRESENTATION_ITEM ( '' )  SURFACE ( )  );
#15796 = ORIENTED_EDGE ( 'NONE', *, *, #5106, .T. ) ;
#15797 = ORIENTED_EDGE ( 'NONE', *, *, #2157, .T. ) ;
#15798 = EDGE_LOOP ( 'NONE', ( #18270, #3241, #12258, #3460 ) ) ;
#15799 = CYLINDRICAL_SURFACE ( 'NONE', #20849, 2.550000000000002043 ) ;
#15800 = DIRECTION ( 'NONE',  ( 0.000000000000000000, 0.000000000000000000, -1.000000000000000000 ) ) ;
#15801 = ORIENTED_EDGE ( 'NONE', *, *, #16294, .F. ) ;
#15802 = DIRECTION ( 'NONE',  ( -1.000000000000000000, 1.700709290173333260E-16, 0.000000000000000000 ) ) ;
#15803 = CARTESIAN_POINT ( 'NONE',  ( 25.00000000000000355, 2.000000000000001776, 0.000000000000000000 ) ) ;
#15804 = DIRECTION ( 'NONE',  ( -1.000000000000000000, -2.699383410053119644E-30, -3.330669073875432643E-16 ) ) ;
#15805 = CARTESIAN_POINT ( 'NONE',  ( 0.000000000000000000, 0.000000000000000000, 0.000000000000000000 ) ) ;
#15806 = CIRCLE ( 'NONE', #8691, 2.550000000000000266 ) ;
#15807 = CIRCLE ( 'NONE', #6070, 2.550000000000010481 ) ;
#15808 = CARTESIAN_POINT ( 'NONE',  ( -6.495190528383341544, 4.999999999999920952, 3.750000000000017319 ) ) ;
#15809 = DIRECTION ( 'NONE',  ( 0.2405376366294550983, 0.000000000000000000, -0.9706398123736303951 ) ) ;
#15810 = DIRECTION ( 'NONE',  ( -0.6819983600625081355, -0.7313537016191615781, 0.000000000000000000 ) ) ;
#15811 = ADVANCED_FACE ( 'NONE', ( #17793 ), #11038, .T. ) ;
#15812 = FACE_OUTER_BOUND ( 'NONE', #2878, .T. ) ;
#15813 = CARTESIAN_POINT ( 'NONE',  ( 3.951447005078454477, 3.704664227300094481, -0.5833333333333537984 ) ) ;
#15814 = CARTESIAN_POINT ( 'NONE',  ( 3.191035955565519888, 1.584759246591017634, 3.972963596181424695 ) ) ;
#15815 = CARTESIAN_POINT ( 'NONE',  ( 77.42435809754130105, -10.99999999999981526, 6.000000000000123457 ) ) ;
#15816 = ORIENTED_EDGE ( 'NONE', *, *, #14388, .F. ) ;
#15817 = EDGE_CURVE ( 'NONE', #22680, #19728, #3977, .T. ) ;
#15818 = CARTESIAN_POINT ( 'NONE',  ( 37.00000000000017053, 0.5000000000000004441, -6.499999999999964473 ) ) ;
#15819 = CARTESIAN_POINT ( 'NONE',  ( 114.8016533820240568, -5.880524088665878502, -6.499999999999970690 ) ) ;
#15820 = EDGE_CURVE ( 'NONE', #2725, #19136, #11328, .T. ) ;
#15822 = ORIENTED_EDGE ( 'NONE', *, *, #21293, .T. ) ;
#15821 = EDGE_LOOP ( 'NONE', ( #11180, #9887, #19901, #3826 ) ) ;
#15823 = EDGE_CURVE ( 'NONE', #3915, #1999, #445, .T. ) ;
#15824 = ORIENTED_EDGE ( 'NONE', *, *, #12556, .T. ) ;
#15825 = AXIS2_PLACEMENT_3D ( 'NONE', #6315, #20548, #18779 ) ;
#15826 = VERTEX_POINT ( 'NONE', #2220 ) ;
#15827 = CARTESIAN_POINT ( 'NONE',  ( 65.19008977971681418, -5.151578709798015687, 6.500000000000179412 ) ) ;
#15828 = CARTESIAN_POINT ( 'NONE',  ( 0.2499999999999898137, 1.500000000000029088, -17.00000000000000711 ) ) ;
#15829 = B_SPLINE_CURVE_WITH_KNOTS ( 'NONE', 3,
 ( #3639, #1861, #9045, #10466 ),
 .UNSPECIFIED., .F., .F.,
 ( 4, 4 ),
 ( 2.380735702043732148E-07, 0.002775112046897002492 ),
 .UNSPECIFIED. ) ;
#15830 = CARTESIAN_POINT ( 'NONE',  ( 7.499999999999978684, -1.390227771353540920, 9.250000000000021316 ) ) ;
#15831 = CARTESIAN_POINT ( 'NONE',  ( 3.974175853610035780, 3.450041667725636252, -1.156004144284049850 ) ) ;
#15832 = EDGE_CURVE ( 'NONE', #22878, #23201, #5713, .T. ) ;
#15833 = DIRECTION ( 'NONE',  ( -1.000000000000000000, 0.000000000000000000, 0.000000000000000000 ) ) ;
#15834 = ADVANCED_FACE ( 'NONE', ( #8614 ), #21451, .T. ) ;
#15835 = CARTESIAN_POINT ( 'NONE',  ( -6.000000000000074607, 5.299999999999964295, 7.500000000000062172 ) ) ;
#15836 = CARTESIAN_POINT ( 'NONE',  ( 2.918498775983380256E-10, -9.961476088449217059E-10, 0.000000000000000000 ) ) ;
#15837 = DIRECTION ( 'NONE',  ( 1.000000000000000000, -7.100545512326564696E-57, -1.066786462891689527E-26 ) ) ;
#15838 = LINE ( 'NONE', #19380, #8162 ) ;
#15839 = CARTESIAN_POINT ( 'NONE',  ( -7.499999999999978684, -8.000000000000010658, 10.74999999999999645 ) ) ;
#15840 = CARTESIAN_POINT ( 'NONE',  ( 42.00000000000020606, 2.999999999999999112, -15.50000000000004086 ) ) ;
#15841 = AXIS2_PLACEMENT_3D ( 'NONE', #12429, #19612, #2071 ) ;
#15842 = CARTESIAN_POINT ( 'NONE',  ( -12.85000000000001386, -12.00000000000005151, 2.550000000000038902 ) ) ;
#15843 = CARTESIAN_POINT ( 'NONE',  ( -55.25320565519145788, 2.700000000000098321, 10.00000000000009237 ) ) ;
#15844 = SURFACE_STYLE_USAGE ( .BOTH. , #16192 ) ;
#15845 = ADVANCED_FACE ( 'NONE', ( #350 ), #19428, .T. ) ;
#15846 = DIRECTION ( 'NONE',  ( -1.000000000000000000, 4.615739097524200579E-16, 1.134196829589820086E-15 ) ) ;
#15847 = ORIENTED_EDGE ( 'NONE', *, *, #4829, .T. ) ;
#15848 = ADVANCED_FACE ( 'NONE', ( #10494 ), #17662, .F. ) ;
#15849 = ORIENTED_EDGE ( 'NONE', *, *, #52, .F. ) ;
#15850 = CARTESIAN_POINT ( 'NONE',  ( -5.423466998235942249, 35.99999999900384751, -25.65320998347783288 ) ) ;
#15852 = EDGE_LOOP ( 'NONE', ( #18525, #1401, #20301, #10062 ) ) ;
#15851 = ORIENTED_EDGE ( 'NONE', *, *, #3077, .T. ) ;
#15853 = AXIS2_PLACEMENT_3D ( 'NONE', #5597, #21251, #1584 ) ;
#15854 = CARTESIAN_POINT ( 'NONE',  ( 0.6640947660599267888, -4.471078309994690692, -3.602146406945891943 ) ) ;
#15855 = CARTESIAN_POINT ( 'NONE',  ( -43.10883117545713361, -4.565685424949276872, 8.000000000000035527 ) ) ;
#15856 = CYLINDRICAL_SURFACE ( 'NONE', #7352, 4.499999999999988454 ) ;
#15857 = CIRCLE ( 'NONE', #2350, 3.499999999999999556 ) ;
#15858 = FACE_OUTER_BOUND ( 'NONE', #19248, .T. ) ;
#15859 = EDGE_CURVE ( 'NONE', #19001, #10962, #3451, .T. ) ;
#15860 = EDGE_LOOP ( 'NONE', ( #1208, #10050, #19632, #3242, #9336, #9535 ) ) ;
#15861 = DIRECTION ( 'NONE',  ( 0.7071067811865474617, -0.7071067811865474617, 0.000000000000000000 ) ) ;
#15862 = DIRECTION ( 'NONE',  ( 1.000000000000000000, 0.000000000000000000, 4.336808689941968432E-16 ) ) ;
#15863 = DIRECTION ( 'NONE',  ( 1.000000000000000000, 0.000000000000000000, 0.000000000000000000 ) ) ;
#15864 = PRODUCT_DEFINITION_SHAPE ( 'NONE', 'NONE',  #23279 ) ;
#15865 = CARTESIAN_POINT ( 'NONE',  ( 1.999999999999953149, -3.464101615137771262, 0.000000000000000000 ) ) ;
#15866 = DIRECTION ( 'NONE',  ( -1.550910762415566494E-16, -1.000000000000000000, 8.135128085091684243E-31 ) ) ;
#15867 = PLANE ( 'NONE',  #1671 ) ;
#15868 = CARTESIAN_POINT ( 'NONE',  ( 4.180345304246196214, -2.049116244671368658, 3.591763845239293484 ) ) ;
#15869 = EDGE_CURVE ( 'NONE', #19838, #21118, #12456, .T. ) ;
#15870 = DIRECTION ( 'NONE',  ( -1.000000000000000000, -4.252453317207022018E-31, 5.551115123125818447E-17 ) ) ;
#15871 = CIRCLE ( 'NONE', #18901, 0.2500000000000002220 ) ;
#15872 = CIRCLE ( 'NONE', #18903, 7.882182279042429407 ) ;
#15873 = TOROIDAL_SURFACE ( 'NONE', #18511, 5.500000000000000000, 0.5000000000000000000 ) ;
#15874 = ORIENTED_EDGE ( 'NONE', *, *, #3924, .T. ) ;
#15875 = CONICAL_SURFACE ( 'NONE', #18907, 3.499999999999999556, 1.047197551196600074 ) ;
#15876 = DIRECTION ( 'NONE',  ( 0.5804539248959940112, 0.8142930928559050097, 1.112876117486888642E-11 ) ) ;
#15877 = EDGE_CURVE ( 'NONE', #21725, #6466, #2318, .T. ) ;
#15879 = VERTEX_POINT ( 'NONE', #9628 ) ;
#15878 = ORIENTED_EDGE ( 'NONE', *, *, #10158, .F. ) ;
#15880 = ORIENTED_EDGE ( 'NONE', *, *, #2635, .F. ) ;
#15882 = ORIENTED_EDGE ( 'NONE', *, *, #353, .F. ) ;
#15881 = VERTEX_POINT ( 'NONE', #22449 ) ;
#15883 = ORIENTED_EDGE ( 'NONE', *, *, #14407, .T. ) ;
#15884 = CARTESIAN_POINT ( 'NONE',  ( -6.219322015043643681, 35.99999999900386172, -26.00774760879520642 ) ) ;
#15885 = CARTESIAN_POINT ( 'NONE',  ( -4.211140560182305315, -2.431303136016589761, -3.745885042887437510 ) ) ;
#15886 = DIRECTION ( 'NONE',  ( 3.885780586188016830E-16, 4.437342591868156373E-31, -1.000000000000000000 ) ) ;
#15887 = AXIS2_PLACEMENT_3D ( 'NONE', #9759, #17264, #1170 ) ;
#15888 = DIRECTION ( 'NONE',  ( -2.172745813409349776E-17, 1.000000000000000000, -1.309377075419428048E-16 ) ) ;
#15889 = VECTOR ( 'NONE', #19292, 1000.000000000000114 ) ;
#15890 = DIRECTION ( 'NONE',  ( 0.5000000000000006661, -2.269329254444893839E-16, -0.8660254037844382635 ) ) ;
#15891 = LINE ( 'NONE', #23104, #17663 ) ;
#15892 = VECTOR ( 'NONE', #1792, 1000.000000000000000 ) ;
#15893 = CARTESIAN_POINT ( 'NONE',  ( 4.663920909892617317, -0.7499999999999384936, -2.263164618243533432 ) ) ;
#15894 = AXIS2_PLACEMENT_3D ( 'NONE', #20944, #1301, #8472 ) ;
#15896 = EDGE_CURVE ( 'NONE', #7485, #3212, #15459, .T. ) ;
#15895 = AXIS2_PLACEMENT_3D ( 'NONE', #13793, #16008, #19087 ) ;
#15897 = DIRECTION ( 'NONE',  ( 0.000000000000000000, -0.000000000000000000, 1.000000000000000000 ) ) ;
#15898 = DIRECTION ( 'NONE',  ( -1.000000000000000000, 1.865174681370276872E-14, -3.854941057726193231E-16 ) ) ;
#15899 = DIRECTION ( 'NONE',  ( 1.333893503340774882E-15, 2.778352770573747380E-17, 1.000000000000000000 ) ) ;
#15900 = CARTESIAN_POINT ( 'NONE',  ( -12.84999999999999964, -13.50000000000003020, 5.750000000000032863 ) ) ;
#15901 = EDGE_CURVE ( 'NONE', #10886, #4366, #20693, .T. ) ;
#15902 = DIRECTION ( 'NONE',  ( -2.013525853228507892E-32, -6.902532920683810383E-31, 1.000000000000000000 ) ) ;
#15903 = DIRECTION ( 'NONE',  ( 3.254448077146059901E-32, 1.000000000000000000, 6.409494854920712161E-31 ) ) ;
#15904 = CARTESIAN_POINT ( 'NONE',  ( 2.000784234979076174E-16, -11.33467790002633357, 7.208584908080428733 ) ) ;
#15905 = CARTESIAN_POINT ( 'NONE',  ( -12.84999999999999964, -12.50000000000011191, -5.749999999999936051 ) ) ;
#15906 = ADVANCED_FACE ( 'NONE', ( #11381 ), #9510, .T. ) ;
#15907 = ORIENTED_EDGE ( 'NONE', *, *, #9880, .F. ) ;
#15908 = AXIS2_PLACEMENT_3D ( 'NONE', #219, #14551, #2080 ) ;
#15909 = AXIS2_PLACEMENT_3D ( 'NONE', #7442, #7112, #21800 ) ;
#15911 = VERTEX_POINT ( 'NONE', #6102 ) ;
#15910 = ORIENTED_EDGE ( 'NONE', *, *, #14109, .F. ) ;
#15912 = VECTOR ( 'NONE', #14657, 1000.000000000000000 ) ;
#15913 = ORIENTED_EDGE ( 'NONE', *, *, #14247, .T. ) ;
#15915 = ORIENTED_EDGE ( 'NONE', *, *, #12972, .T. ) ;
#15914 = ORIENTED_EDGE ( 'NONE', *, *, #7173, .T. ) ;
#15916 = VERTEX_POINT ( 'NONE', #13164 ) ;
#15917 = ORIENTED_EDGE ( 'NONE', *, *, #8666, .F. ) ;
#15918 = DIRECTION ( 'NONE',  ( 0.000000000000000000, 1.000000000000000000, 0.000000000000000000 ) ) ;
#15919 = FACE_OUTER_BOUND ( 'NONE', #22063, .T. ) ;
#15920 = ORIENTED_EDGE ( 'NONE', *, *, #14300, .T. ) ;
#15921 = CYLINDRICAL_SURFACE ( 'NONE', #1508, 7.200000000000046363 ) ;
#15922 = CARTESIAN_POINT ( 'NONE',  ( -6.938893903861184144E-14, 4.999999999999976907, -4.750000000000041744 ) ) ;
#15923 = TOROIDAL_SURFACE ( 'NONE', #5813, 1.750000000000000000, 0.2500000000000000000 ) ;
#15924 = B_SPLINE_CURVE_WITH_KNOTS ( 'NONE', 3,
 ( #12294, #3382, #10541, #13349, #11454, #17322, #20531, #4276, #9937, #20648, #22634, #6293, #17088, #2991, #11570, #10161, #6409, #18756 ),
 .UNSPECIFIED., .F., .F.,
 ( 4, 2, 2, 2, 2, 2, 2, 2, 4 ),
 ( 0.000000000000000000, 0.0005979442104825547725, 0.001195888420965109545, 0.001793832631447664317, 0.002391776841930219090, 0.002989721052412773646, 0.003587665262895328635, 0.004185609473377883624, 0.004783553683860438180 ),
 .UNSPECIFIED. ) ;
#15925 = CARTESIAN_POINT ( 'NONE',  ( 54.42435809754118736, 2.999999999999947153, -6.499999999999922728 ) ) ;
#15926 = CLOSED_SHELL ( 'NONE', ( #14125, #10220, #15400, #19594, #19134, #4506, #12570, #15994, #20613, #6835, #18562, #9770, #10453, #18324, #12084 ) ) ;
#15927 = AXIS2_PLACEMENT_3D ( 'NONE', #11995, #3071, #15411 ) ;
#15928 = DIRECTION ( 'NONE',  ( -0.000000000000000000, 0.000000000000000000, -1.000000000000000000 ) ) ;
#15929 = CARTESIAN_POINT ( 'NONE',  ( -3.200000000000119194, -6.938893903907228378E-14, 7.500000000000062172 ) ) ;
#15930 = CARTESIAN_POINT ( 'NONE',  ( 54.42435809754113052, -4.000000000000003553, -6.000000000000012434 ) ) ;
#15931 = AXIS2_PLACEMENT_3D ( 'NONE', #17458, #5241, #19577 ) ;
#15932 = DIRECTION ( 'NONE',  ( -5.551115123125796261E-17, 0.000000000000000000, 1.000000000000000000 ) ) ;
#15933 = PRESENTATION_STYLE_ASSIGNMENT (( #19719 ) ) ;
#15934 = DIRECTION ( 'NONE',  ( 1.454462294001240516E-30, 1.000000000000000000, 0.000000000000000000 ) ) ;
#15935 = CARTESIAN_POINT ( 'NONE',  ( 4.113620667976089607, 1.749999999999973799, 2.375000000000000444 ) ) ;
#15936 = CARTESIAN_POINT ( 'NONE',  ( 66.26395429947839943, -7.000000000000006217, -6.000000000000060396 ) ) ;
#15937 = ORIENTED_EDGE ( 'NONE', *, *, #8834, .T. ) ;
#15938 = CARTESIAN_POINT ( 'NONE',  ( 108.2426266706970353, -13.02760560296359316, -6.000000000000019540 ) ) ;
#15939 = DIRECTION ( 'NONE',  ( -1.000000000000000000, -1.479114197289397135E-31, -5.916456789157588541E-31 ) ) ;
#15941 = ORIENTED_EDGE ( 'NONE', *, *, #15331, .T. ) ;
#15940 = VERTEX_POINT ( 'NONE', #6221 ) ;
#15942 = PRODUCT_RELATED_PRODUCT_CATEGORY ( 'part', '', ( #14203 ) ) ;
#15943 = AXIS2_PLACEMENT_3D ( 'NONE', #10585, #7187, #12343 ) ;
#15944 = EDGE_LOOP ( 'NONE', ( #14674, #16174, #4406, #15396 ) ) ;
#15945 = APPLICATION_CONTEXT ( 'automotive_design' ) ;
#15946 = VERTEX_POINT ( 'NONE', #698 ) ;
#15947 = ORIENTED_EDGE ( 'NONE', *, *, #17555, .T. ) ;
#15948 = EDGE_CURVE ( 'NONE', #6218, #20629, #11271, .T. ) ;
#15949 = CARTESIAN_POINT ( 'NONE',  ( 2.775557561562891351E-14, 8.500000000000003553, -12.50000000000001066 ) ) ;
#15950 = FACE_OUTER_BOUND ( 'NONE', #14396, .T. ) ;
#15951 = CARTESIAN_POINT ( 'NONE',  ( 12.84999999999995879, 0.000000000000000000, 5.749999999999991118 ) ) ;
#15952 = CARTESIAN_POINT ( 'NONE',  ( 42.00000000000014921, 5.500000000000001776, -15.00000000000001421 ) ) ;
#15953 = ADVANCED_FACE ( 'NONE', ( #4317 ), #18568, .F. ) ;
#15954 = DIRECTION ( 'NONE',  ( 1.000000000000000000, 0.000000000000000000, 0.000000000000000000 ) ) ;
#15955 = CARTESIAN_POINT ( 'NONE',  ( 5.600000000000000533, 4.041451884327335264, -1.734723475976807094E-14 ) ) ;
#15956 = DIRECTION ( 'NONE',  ( 1.454462294001240516E-30, 1.000000000000000000, 0.000000000000000000 ) ) ;
#15957 = PLANE ( 'NONE',  #16724 ) ;
#15958 = FACE_OUTER_BOUND ( 'NONE', #10909, .T. ) ;
#15959 = VECTOR ( 'NONE', #12434, 1000.000000000000000 ) ;
#15960 = CARTESIAN_POINT ( 'NONE',  ( -6.000000000000143885, -2.000000000000043521, 8.000000000000062172 ) ) ;
#15961 = VECTOR ( 'NONE', #1302, 1000.000000000000000 ) ;
#15962 = DIRECTION ( 'NONE',  ( -8.438582421954109416E-32, 0.000000000000000000, -1.000000000000000000 ) ) ;
#15963 = CYLINDRICAL_SURFACE ( 'NONE', #2141, 0.5000000000000004441 ) ;
#15964 = DIRECTION ( 'NONE',  ( -2.013525853228507892E-32, -6.902532920683810383E-31, 1.000000000000000000 ) ) ;
#15965 = CARTESIAN_POINT ( 'NONE',  ( -7.499999999999992895, -6.999999999999995559, 11.74999999999999645 ) ) ;
#15966 = ORIENTED_EDGE ( 'NONE', *, *, #6206, .T. ) ;
#15967 = ADVANCED_FACE ( 'NONE', ( #16779 ), #12075, .T. ) ;
#15968 = EDGE_LOOP ( 'NONE', ( #13420, #112, #21588, #17657, #16322, #10089, #422, #10392 ) ) ;
#15969 = EDGE_CURVE ( 'NONE', #1774, #2242, #2328, .T. ) ;
#15970 = DIRECTION ( 'NONE',  ( 1.000000000000000000, -1.389842848855773151E-62, 2.013525853228507618E-32 ) ) ;
#15972 = ORIENTED_EDGE ( 'NONE', *, *, #8838, .F. ) ;
#15971 = ORIENTED_EDGE ( 'NONE', *, *, #1959, .T. ) ;
#15973 = CIRCLE ( 'NONE', #6992, 2.500000000000002220 ) ;
#15974 = CARTESIAN_POINT ( 'NONE',  ( 4.141042297810574091, -2.227970268150456068, -3.687027686973618934 ) ) ;
#15975 = DIRECTION ( 'NONE',  ( 2.013525853228507892E-32, 6.902532920683810383E-31, -1.000000000000000000 ) ) ;
#15976 = DIRECTION ( 'NONE',  ( -1.000000000000000000, -1.479114197289397135E-31, -5.916456789157588541E-31 ) ) ;
#15977 =( NAMED_UNIT ( * ) SI_UNIT ( $, .STERADIAN. ) SOLID_ANGLE_UNIT ( ) );
#15979 = ORIENTED_EDGE ( 'NONE', *, *, #3328, .T. ) ;
#15978 = EDGE_CURVE ( 'NONE', #15576, #22415, #4947, .T. ) ;
#15980 = AXIS2_PLACEMENT_3D ( 'NONE', #5676, #3890, #3667 ) ;
#15981 = CARTESIAN_POINT ( 'NONE',  ( -2.000000000000036415, 3.464101615137757495, 0.000000000000000000 ) ) ;
#15982 = CARTESIAN_POINT ( 'NONE',  ( 0.000000000000000000, 0.000000000000000000, -5.000000000000000888 ) ) ;
#15983 = EDGE_CURVE ( 'NONE', #10216, #522, #831, .T. ) ;
#15984 = DIRECTION ( 'NONE',  ( -2.220446049250313081E-16, 1.000000000000000000, -7.025792437124636392E-31 ) ) ;
#15985 = EDGE_CURVE ( 'NONE', #22677, #19900, #2808, .T. ) ;
#15986 = CARTESIAN_POINT ( 'NONE',  ( 78.36587326203826365, -2.990348597579628454, -6.499999999999984901 ) ) ;
#15987 = DIRECTION ( 'NONE',  ( -1.000000000000000000, 4.190823558986610327E-31, -1.733449886265890494E-32 ) ) ;
#15988 = CARTESIAN_POINT ( 'NONE',  ( -4.000000000000098588, -0.7890432684750791070, -0.04868663549888898462 ) ) ;
#15989 = DIRECTION ( 'NONE',  ( -0.2405376366294452728, 0.000000000000000000, 0.9706398123736327266 ) ) ;
#15990 = DIRECTION ( 'NONE',  ( -1.756300210255732376E-61, 4.190823558986625216E-31, 1.000000000000000000 ) ) ;
#15991 = CARTESIAN_POINT ( 'NONE',  ( 5.600000000000000533, 0.000000000000000000, -3.469446951953614189E-15 ) ) ;
#15992 = CARTESIAN_POINT ( 'NONE',  ( -1.030839096808483710E-15, -0.3420925509533346287, 3.499999999999994227 ) ) ;
#15993 = PRESENTATION_STYLE_ASSIGNMENT (( #3317 ) ) ;
#15994 = ADVANCED_FACE ( 'NONE', ( #20573, #5993 ), #20336, .T. ) ;
#15995 = VERTEX_POINT ( 'NONE', #20228 ) ;
#15996 = EDGE_CURVE ( 'NONE', #18159, #22993, #6106, .T. ) ;
#15997 = ADVANCED_FACE ( 'NONE', ( #22921, #21154 ), #14086, .T. ) ;
#15998 = AXIS2_PLACEMENT_3D ( 'NONE', #17756, #13992, #7178 ) ;
#15999 = DIRECTION ( 'NONE',  ( 1.000000000000000000, 9.714451465470117757E-16, 9.714451465470133534E-16 ) ) ;
#16001 = ORIENTED_EDGE ( 'NONE', *, *, #13524, .F. ) ;
#16000 = ORIENTED_EDGE ( 'NONE', *, *, #17720, .T. ) ;
#16002 = EDGE_LOOP ( 'NONE', ( #2884, #23122, #2413, #4530, #22385 ) ) ;
#16004 = VERTEX_POINT ( 'NONE', #10554 ) ;
#16003 = VERTEX_POINT ( 'NONE', #19256 ) ;
#16005 = EDGE_CURVE ( 'NONE', #6667, #4783, #20015, .T. ) ;
#16006 = CARTESIAN_POINT ( 'NONE',  ( -4.773379239211062774, 35.99999999900384751, -25.50000000000000355 ) ) ;
#16007 = DIRECTION ( 'NONE',  ( -1.333893503340774882E-15, -2.778352770573747380E-17, -1.000000000000000000 ) ) ;
#16008 = DIRECTION ( 'NONE',  ( -1.000000000000000000, -2.699383410053119644E-30, -3.330669073875432643E-16 ) ) ;
#16009 = DIRECTION ( 'NONE',  ( -1.000000000000000000, 0.000000000000000000, 0.000000000000000000 ) ) ;
#16010 = EDGE_CURVE ( 'NONE', #2292, #4567, #6468, .T. ) ;
#16011 = DIRECTION ( 'NONE',  ( -2.753132232808522832E-17, 0.6666666666666728469, 0.7453559924999245689 ) ) ;
#16012 = CARTESIAN_POINT ( 'NONE',  ( 4.630153689607049650, 0.000000000000000000, -3.469446951953614189E-15 ) ) ;
#16013 = CARTESIAN_POINT ( 'NONE',  ( 7.644579933246805403, -13.15747815713138991, 8.321099285265846746 ) ) ;
#16014 = FILL_AREA_STYLE_COLOUR ( '', #6735 ) ;
#16015 = CARTESIAN_POINT ( 'NONE',  ( -55.25320565519145788, 0.5000000000000905942, 10.00000000000009237 ) ) ;
#16016 = DIRECTION ( 'NONE',  ( 4.313844246609350428E-33, 6.982962677686276966E-15, 1.000000000000000000 ) ) ;
#16017 = CARTESIAN_POINT ( 'NONE',  ( -95.70000000000058549, -2.700000000000119194, 1.000000000000014655 ) ) ;
#16018 = CARTESIAN_POINT ( 'NONE',  ( 2.775557561562891351E-14, 2.999999999999992450, -0.4999999999999865663 ) ) ;
#16019 = AXIS2_PLACEMENT_3D ( 'NONE', #4420, #4542, #1260 ) ;
#16020 = DIRECTION ( 'NONE',  ( 1.000000000000000000, 0.000000000000000000, 0.000000000000000000 ) ) ;
#16021 = DIRECTION ( 'NONE',  ( -1.000000000000000000, -2.220446049250301001E-16, 0.000000000000000000 ) ) ;
#16022 = CIRCLE ( 'NONE', #18666, 0.4999999999999999445 ) ;
#16023 = EDGE_CURVE ( 'NONE', #4862, #5668, #20926, .T. ) ;
#16024 = DIRECTION ( 'NONE',  ( 1.000000000000000000, 2.699383410053119644E-30, 3.330669073875432643E-16 ) ) ;
#16025 = ORIENTED_EDGE ( 'NONE', *, *, #7180, .F. ) ;
#16027 = ORIENTED_EDGE ( 'NONE', *, *, #5371, .T. ) ;
#16026 = EDGE_LOOP ( 'NONE', ( #13617, #15618 ) ) ;
#16028 = VERTEX_POINT ( 'NONE', #10200 ) ;
#16030 = ORIENTED_EDGE ( 'NONE', *, *, #23196, .T. ) ;
#16029 = EDGE_LOOP ( 'NONE', ( #14390, #12918, #1181, #1354 ) ) ;
#16031 = ORIENTED_EDGE ( 'NONE', *, *, #67, .T. ) ;
#16032 = AXIS2_PLACEMENT_3D ( 'NONE', #14958, #22139, #6030 ) ;
#16033 = ORIENTED_EDGE ( 'NONE', *, *, #17733, .T. ) ;
#16034 = VERTEX_POINT ( 'NONE', #6683 ) ;
#16035 = DIRECTION ( 'NONE',  ( 0.9706398123736300620, 1.281898970984135951E-30, 0.2405376366294562085 ) ) ;
#16036 = VECTOR ( 'NONE', #11649, 1000.000000000000000 ) ;
#16037 = AXIS2_PLACEMENT_3D ( 'NONE', #21803, #18381, #2257 ) ;
#16038 = CARTESIAN_POINT ( 'NONE',  ( -3.414274948570356294, 6.938893903907228378E-14, -21.66938530120590656 ) ) ;
#16039 = CARTESIAN_POINT ( 'NONE',  ( -2.681483223904243207, 3.070647092368421927, 2.148523566439784158E-15 ) ) ;
#16040 = EDGE_CURVE ( 'NONE', #15168, #6539, #1504, .T. ) ;
#16041 = CARTESIAN_POINT ( 'NONE',  ( -89.70000000000055707, -2.700000000000084110, -1.999999999999946265 ) ) ;
#16042 = VECTOR ( 'NONE', #20702, 1000.000000000000000 ) ;
#16043 = CARTESIAN_POINT ( 'NONE',  ( 36.00000000029184832, 2.999999999003851503, 0.000000000000000000 ) ) ;
#16044 = DIRECTION ( 'NONE',  ( 1.000000000000000000, 0.000000000000000000, 0.000000000000000000 ) ) ;
#16045 = CARTESIAN_POINT ( 'NONE',  ( 6.000000000291855429, 2.999999999003851503, -39.00000000000000000 ) ) ;
#16046 = CARTESIAN_POINT ( 'NONE',  ( 2.000000000000015543, -3.464101615137746837, -5.600000000000000533 ) ) ;
#16047 = CARTESIAN_POINT ( 'NONE',  ( -6.359599319592075695, 13.97158350606811617, -17.13641408681294109 ) ) ;
#16048 = CIRCLE ( 'NONE', #6679, 4.500000000000031974 ) ;
#16049 = CARTESIAN_POINT ( 'NONE',  ( -65.47859922179024750, -3.200000000000088107, -11.38422848940306942 ) ) ;
#16050 = TOROIDAL_SURFACE ( 'NONE', #2151, 3.500000000000000000, 0.5000000000000000000 ) ;
#16051 = VERTEX_POINT ( 'NONE', #6922 ) ;
#16052 = DIRECTION ( 'NONE',  ( 0.000000000000000000, 0.000000000000000000, 1.000000000000000000 ) ) ;
#16053 = DIRECTION ( 'NONE',  ( 0.000000000000000000, 0.8381404052084411305, -0.5454545454545505212 ) ) ;
#16055 = ORIENTED_EDGE ( 'NONE', *, *, #1358, .T. ) ;
#16054 = ORIENTED_EDGE ( 'NONE', *, *, #4199, .T. ) ;
#16056 = VECTOR ( 'NONE', #14685, 1000.000000000000000 ) ;
#16057 = CIRCLE ( 'NONE', #22087, 0.5000000000000029976 ) ;
#16058 = CIRCLE ( 'NONE', #4042, 2.999999999999995559 ) ;
#16059 = VERTEX_POINT ( 'NONE', #13626 ) ;
#16060 = ORIENTED_EDGE ( 'NONE', *, *, #8222, .F. ) ;
#16061 = ORIENTED_EDGE ( 'NONE', *, *, #7959, .T. ) ;
#16062 = PRODUCT_DEFINITION_SHAPE ( 'NONE', 'NONE',  #23272 ) ;
#16063 = ORIENTED_EDGE ( 'NONE', *, *, #16040, .F. ) ;
#16064 = DIRECTION ( 'NONE',  ( 0.000000000000000000, 0.000000000000000000, -1.000000000000000000 ) ) ;
#16065 = CARTESIAN_POINT ( 'NONE',  ( 7.607945571813329089, -0.8975439866889015628, 8.443122311927325541 ) ) ;
#16066 = CIRCLE ( 'NONE', #19085, 0.5000000000000006661 ) ;
#16067 = CARTESIAN_POINT ( 'NONE',  ( 4.132952817037863547, -2.031684012687259955, -3.518979934899747253 ) ) ;
#16068 = DIRECTION ( 'NONE',  ( 1.000000000000000000, 2.168404344971017743E-16, -1.780660105995169760E-30 ) ) ;
#16069 = CARTESIAN_POINT ( 'NONE',  ( 42.50000000000014921, 2.999999999999999112, -12.49999999999998401 ) ) ;
#16070 = AXIS2_PLACEMENT_3D ( 'NONE', #17256, #17024, #10323 ) ;
#16071 = DIRECTION ( 'NONE',  ( 1.000000000000000000, -2.168404344971017743E-16, 1.203141491611691375E-30 ) ) ;
#16072 = DIRECTION ( 'NONE',  ( 0.000000000000000000, -1.000000000000000000, 0.000000000000000000 ) ) ;
#16073 = CYLINDRICAL_SURFACE ( 'NONE', #20717, 0.4999999999999987232 ) ;
#16074 = AXIS2_PLACEMENT_3D ( 'NONE', #21662, #16218, #21315 ) ;
#16075 = DIRECTION ( 'NONE',  ( 1.000000000000000000, 0.000000000000000000, 0.000000000000000000 ) ) ;
#16076 = AXIS2_PLACEMENT_3D ( 'NONE', #21661, #5186, #19534 ) ;
#16077 = CARTESIAN_POINT ( 'NONE',  ( 0.000000000000000000, -1.750000000000001554, 0.000000000000000000 ) ) ;
#16078 = CARTESIAN_POINT ( 'NONE',  ( -4.113620667976075396, 1.749999999999998002, 2.374999999999998668 ) ) ;
#16079 =( NAMED_UNIT ( * ) PLANE_ANGLE_UNIT ( ) SI_UNIT ( $, .RADIAN. ) );
#16080 = EDGE_CURVE ( 'NONE', #15636, #19862, #11340, .T. ) ;
#16081 = CARTESIAN_POINT ( 'NONE',  ( 24.74999999999996447, 1.500000000000043077, -2.081668171172168513E-14 ) ) ;
#16082 = CARTESIAN_POINT ( 'NONE',  ( 30.00000000029184832, 2.999999999003851503, 0.000000000000000000 ) ) ;
#16083 = ORIENTED_EDGE ( 'NONE', *, *, #15029, .T. ) ;
#16084 = ORIENTED_EDGE ( 'NONE', *, *, #15566, .T. ) ;
#16085 = B_SPLINE_CURVE_WITH_KNOTS ( 'NONE', 3,
 ( #18896, #15697, #17469, #21255 ),
 .UNSPECIFIED., .F., .F.,
 ( 4, 4 ),
 ( 2.380735702001470497E-07, 0.002775112046897012467 ),
 .UNSPECIFIED. ) ;
#16086 = CARTESIAN_POINT ( 'NONE',  ( -56.87767137932630845, 0.5000000000000905942, 8.833333333333415638 ) ) ;
#16087 = AXIS2_PLACEMENT_3D ( 'NONE', #4184, #12914, #2083 ) ;
#16088 = VERTEX_POINT ( 'NONE', #8328 ) ;
#16089 = CIRCLE ( 'NONE', #14596, 5.500000000000000000 ) ;
#16090 = EDGE_CURVE ( 'NONE', #396, #16375, #22566, .T. ) ;
#16091 = CARTESIAN_POINT ( 'NONE',  ( -3.880358743661276755, -1.739972214219213109, -2.779021504384352248 ) ) ;
#16092 = CARTESIAN_POINT ( 'NONE',  ( 4.175813232069149450, 4.122719923832687705, 1.040834085586084257E-14 ) ) ;
#16093 = SURFACE_SIDE_STYLE ('',( #1981 ) ) ;
#16094 = VERTEX_POINT ( 'NONE', #12066 ) ;
#16095 = CARTESIAN_POINT ( 'NONE',  ( 0.1397371499201390255, 1.362866705336802875, 3.499999999999957812 ) ) ;
#16096 = DIRECTION ( 'NONE',  ( -0.7313537016191746787, 0.6819983600624941467, 5.177789255530095281E-17 ) ) ;
#16097 = CARTESIAN_POINT ( 'NONE',  ( 27.94974746859769255, 27.94974746730969528, -19.49999999999998934 ) ) ;
#16098 = PRESENTATION_LAYER_ASSIGNMENT (  '', '', ( #338 ) ) ;
#16099 = CARTESIAN_POINT ( 'NONE',  ( 1.200000000000006617, -0.5999999999999963141, -4.543283425070376857 ) ) ;
#16100 = CARTESIAN_POINT ( 'NONE',  ( 4.175075985190096262, 2.060370777630105010, -3.568666869285575860 ) ) ;
#16101 = CARTESIAN_POINT ( 'NONE',  ( 4.030867648404789172, -2.329326259789488596, 2.965488570641482191 ) ) ;
#16102 = PRESENTATION_STYLE_ASSIGNMENT (( #9182 ) ) ;
#16103 = EDGE_CURVE ( 'NONE', #19898, #11147, #20819, .T. ) ;
#16104 = AXIS2_PLACEMENT_3D ( 'NONE', #21721, #5720, #13123 ) ;
#16105 = CARTESIAN_POINT ( 'NONE',  ( 3.999999999999939160, 0.3987449864459891025, -0.01220643443054973340 ) ) ;
#16106 = CONICAL_SURFACE ( 'NONE', #6357, 3.499999999999999556, 1.047197551196600074 ) ;
#16107 =( NAMED_UNIT ( * ) PLANE_ANGLE_UNIT ( ) SI_UNIT ( $, .RADIAN. ) );
#16108 = ORIENTED_EDGE ( 'NONE', *, *, #21414, .F. ) ;
#16109 = EDGE_CURVE ( 'NONE', #8762, #12385, #5145, .T. ) ;
#16110 = DIRECTION ( 'NONE',  ( -0.2080827065197027592, -0.9781112345983126177, 2.870775330660612664E-16 ) ) ;
#16111 = EDGE_CURVE ( 'NONE', #8379, #14963, #13854, .T. ) ;
#16113 = ORIENTED_EDGE ( 'NONE', *, *, #5841, .T. ) ;
#16112 = ORIENTED_EDGE ( 'NONE', *, *, #7643, .F. ) ;
#16114 = EDGE_CURVE ( 'NONE', #7007, #10053, #1477, .T. ) ;
#16115 = STYLED_ITEM ( 'NONE', ( #18386 ), #202 ) ;
#16116 = EDGE_LOOP ( 'NONE', ( #2467, #3429, #5729, #9886 ) ) ;
#16118 = VERTEX_POINT ( 'NONE', #10441 ) ;
#16117 = ORIENTED_EDGE ( 'NONE', *, *, #6360, .F. ) ;
#16119 = DIRECTION ( 'NONE',  ( 1.000000000000000000, 0.000000000000000000, 0.000000000000000000 ) ) ;
#16120 = CARTESIAN_POINT ( 'NONE',  ( -4.550510256924974684, 36.49999999900384751, -25.50000000000000000 ) ) ;
#16121 = CARTESIAN_POINT ( 'NONE',  ( -67.28510754798017501, -0.5000000000001045830, 12.22107821754960000 ) ) ;
#16122 = CARTESIAN_POINT ( 'NONE',  ( 35.50000000029184832, 16.99999999900385461, -26.50000000000000000 ) ) ;
#16123 = CARTESIAN_POINT ( 'NONE',  ( -6.962001439796694058, 35.99999999900384751, -18.52402997057235723 ) ) ;
#16124 = ADVANCED_FACE ( 'NONE', ( #4900 ), #12310, .T. ) ;
#16125 = DIRECTION ( 'NONE',  ( 5.551115123561405253E-17, 1.000000000000000000, 2.256980353643891447E-27 ) ) ;
#16127 = EDGE_CURVE ( 'NONE', #5606, #2826, #1955, .T. ) ;
#16126 = DIRECTION ( 'NONE',  ( 0.000000000000000000, 0.000000000000000000, 1.000000000000000000 ) ) ;
#16128 = DIRECTION ( 'NONE',  ( -2.775557561562902444E-17, 0.000000000000000000, -1.000000000000000000 ) ) ;
#16129 = DIRECTION ( 'NONE',  ( -0.7071067811865233699, 0.7071067811865715536, 1.565905175853783930E-16 ) ) ;
#16130 = CIRCLE ( 'NONE', #5627, 0.5000000000000004441 ) ;
#16131 = DIRECTION ( 'NONE',  ( 1.454462294001240516E-30, 1.000000000000000000, 0.000000000000000000 ) ) ;
#16132 = CYLINDRICAL_SURFACE ( 'NONE', #18481, 0.5000000000000017764 ) ;
#16133 = PRODUCT_DEFINITION_FORMATION_WITH_SPECIFIED_SOURCE ( 'ANY', '', #21350, .NOT_KNOWN. ) ;
#16134 = CARTESIAN_POINT ( 'NONE',  ( 31.55000000029185259, 16.99999999900385461, -25.50000000000000355 ) ) ;
#16135 = DIRECTION ( 'NONE',  ( 0.000000000000000000, 6.802837160693368935E-15, 1.000000000000000000 ) ) ;
#16136 = CARTESIAN_POINT ( 'NONE',  ( 2.918498775983380256E-10, 2.999999999003851503, 0.000000000000000000 ) ) ;
#16137 = EDGE_CURVE ( 'NONE', #2880, #2293, #9474, .T. ) ;
#16138 = CARTESIAN_POINT ( 'NONE',  ( 8.697224362267983011, 1.474514954580286030E-14, 6.250000000000023093 ) ) ;
#16139 = ORIENTED_EDGE ( 'NONE', *, *, #13570, .T. ) ;
#16140 = EDGE_CURVE ( 'NONE', #22552, #20884, #7237, .T. ) ;
#16141 = PRESENTATION_STYLE_ASSIGNMENT (( #3235 ) ) ;
#16143 = ORIENTED_EDGE ( 'NONE', *, *, #11685, .F. ) ;
#16142 = EDGE_LOOP ( 'NONE', ( #6626, #22033, #16170, #15678 ) ) ;
#16144 = EDGE_CURVE ( 'NONE', #18229, #20684, #16341, .T. ) ;
#16145 = ORIENTED_EDGE ( 'NONE', *, *, #3766, .T. ) ;
#16147 = EDGE_LOOP ( 'NONE', ( #17786, #15217, #21620, #17956 ) ) ;
#16146 = VERTEX_POINT ( 'NONE', #17725 ) ;
#16148 = CIRCLE ( 'NONE', #401, 4.750000000000013323 ) ;
#16149 =( REPRESENTATION_RELATIONSHIP ('NONE','NONE', #19450, #4439 ) REPRESENTATION_RELATIONSHIP_WITH_TRANSFORMATION ( #11630 )SHAPE_REPRESENTATION_RELATIONSHIP( ) );
#16150 = EDGE_LOOP ( 'NONE', ( #22181, #571, #14860, #274 ) ) ;
#16151 = VERTEX_POINT ( 'NONE', #3721 ) ;
#16152 = ORIENTED_EDGE ( 'NONE', *, *, #2937, .T. ) ;
#16153 = CARTESIAN_POINT ( 'NONE',  ( 0.02842916987967946188, 0.6000000000000131894, 3.398229573760024991 ) ) ;
#16154 = CARTESIAN_POINT ( 'NONE',  ( -50.65685424949267457, -3.200000000000108979, -7.500000000000034639 ) ) ;
#16155 = CARTESIAN_POINT ( 'NONE',  ( -7.786490775660109165, -13.29349257805250595, 7.963863235126091844 ) ) ;
#16156 = CARTESIAN_POINT ( 'NONE',  ( 0.000000000000000000, 0.000000000000000000, 0.000000000000000000 ) ) ;
#16157 = CARTESIAN_POINT ( 'NONE',  ( 6.999999999999992006, -8.000000000000051514, 6.249999999999977796 ) ) ;
#16158 = CARTESIAN_POINT ( 'NONE',  ( 3.951447005078452701, -3.704664227300147328, 0.5833333333333443615 ) ) ;
#16159 = CARTESIAN_POINT ( 'NONE',  ( -3.540020015735878545, -2.810662092924825384, -3.602146406946029611 ) ) ;
#16160 =( NAMED_UNIT ( * ) SI_UNIT ( $, .STERADIAN. ) SOLID_ANGLE_UNIT ( ) );
#16161 = LINE ( 'NONE', #1713, #6688 ) ;
#16162 = AXIS2_PLACEMENT_3D ( 'NONE', #11902, #19089, #17310 ) ;
#16163 = CARTESIAN_POINT ( 'NONE',  ( -57.28378781035996070, 3.200000000000098765, 8.541666666666724694 ) ) ;
#16164 = ADVANCED_FACE ( 'NONE', ( #317 ), #1839, .F. ) ;
#16165 = FACE_BOUND ( 'NONE', #18560, .T. ) ;
#16166 = ORIENTED_EDGE ( 'NONE', *, *, #14205, .T. ) ;
#16167 =( LENGTH_UNIT ( ) NAMED_UNIT ( * ) SI_UNIT ( .MILLI., .METRE. ) );
#16168 = CARTESIAN_POINT ( 'NONE',  ( 0.000000000000000000, 0.000000000000000000, 0.000000000000000000 ) ) ;
#16169 = CARTESIAN_POINT ( 'NONE',  ( -92.25000000000058265, -8.981013850637800498E-14, -2.000000000000001776 ) ) ;
#16171 = ORIENTED_EDGE ( 'NONE', *, *, #10863, .F. ) ;
#16170 = ORIENTED_EDGE ( 'NONE', *, *, #1071, .F. ) ;
#16172 = ADVANCED_FACE ( 'NONE', ( #1727 ), #3952, .T. ) ;
#16173 = EDGE_LOOP ( 'NONE', ( #9652, #13005, #6820, #2524 ) ) ;
#16174 = ORIENTED_EDGE ( 'NONE', *, *, #16127, .F. ) ;
#16175 = VERTEX_POINT ( 'NONE', #14540 ) ;
#16176 = ORIENTED_EDGE ( 'NONE', *, *, #779, .T. ) ;
#16177 = DIRECTION ( 'NONE',  ( 0.9706398123736330597, 2.155253336630096709E-16, 0.2405376366294442736 ) ) ;
#16178 = CIRCLE ( 'NONE', #22578, 4.750000000000013323 ) ;
#16179 = CARTESIAN_POINT ( 'NONE',  ( -0.5000000000000837108, 7.199999999999977085, -8.000000000000007105 ) ) ;
#16180 = ADVANCED_FACE ( 'NONE', ( #12658 ), #7379, .T. ) ;
#16181 = CARTESIAN_POINT ( 'NONE',  ( 0.000000000000000000, 0.000000000000000000, 0.000000000000000000 ) ) ;
#16182 = DIRECTION ( 'NONE',  ( 0.000000000000000000, 0.000000000000000000, 1.000000000000000000 ) ) ;
#16183 = DIRECTION ( 'NONE',  ( -3.032184104443272185E-30, -1.000000000000000000, 7.395570986447005381E-32 ) ) ;
#16184 = DIRECTION ( 'NONE',  ( -0.000000000000000000, -0.000000000000000000, 1.000000000000000000 ) ) ;
#16185 = CARTESIAN_POINT ( 'NONE',  ( 0.3126073911696378160, 2.020725942163612121, 3.499999999999975131 ) ) ;
#16186 = DIRECTION ( 'NONE',  ( -1.000000000000000000, -2.699383410053119644E-30, -3.330669073875432643E-16 ) ) ;
#16187 = CYLINDRICAL_SURFACE ( 'NONE', #17078, 2.549999999999997158 ) ;
#16188 = DIRECTION ( 'NONE',  ( -2.172745813409349776E-17, 1.000000000000000000, -1.309377075419428048E-16 ) ) ;
#16189 = CARTESIAN_POINT ( 'NONE',  ( -6.866595637047972822, -0.5000000000000350830, 27.70872448147272848 ) ) ;
#16190 = DIRECTION ( 'NONE',  ( -2.220446049250313081E-16, 1.000000000000000000, -7.025792437124636392E-31 ) ) ;
#16191 = EDGE_CURVE ( 'NONE', #16369, #11583, #21288, .T. ) ;
#16192 = SURFACE_SIDE_STYLE ('',( #8922 ) ) ;
#16193 = FACE_OUTER_BOUND ( 'NONE', #1913, .T. ) ;
#16195 = AXIS2_PLACEMENT_3D ( 'NONE', #19849, #10894, #9260 ) ;
#16194 = DIRECTION ( 'NONE',  ( -2.013525853228518840E-32, 6.902532920683810383E-31, -1.000000000000000000 ) ) ;
#16196 = ORIENTED_EDGE ( 'NONE', *, *, #626, .T. ) ;
#16197 = EDGE_CURVE ( 'NONE', #9451, #2560, #5695, .T. ) ;
#16198 = ORIENTED_EDGE ( 'NONE', *, *, #12498, .F. ) ;
#16199 = CARTESIAN_POINT ( 'NONE',  ( -3.999999999708154341, 38.75225147438560924, -29.00000000000001066 ) ) ;
#16200 = ORIENTED_EDGE ( 'NONE', *, *, #12953, .F. ) ;
#16201 = CARTESIAN_POINT ( 'NONE',  ( -0.02448733951244273441, -4.877042772274788440, -3.751161874094042226 ) ) ;
#16202 = DIRECTION ( 'NONE',  ( 0.6819983600625060260, 0.7313537016191635765, 6.106365041599011361E-16 ) ) ;
#16203 = FACE_OUTER_BOUND ( 'NONE', #2380, .T. ) ;
#16204 = EDGE_CURVE ( 'NONE', #4397, #6390, #3824, .T. ) ;
#16205 = CARTESIAN_POINT ( 'NONE',  ( 124.5000000000019469, -4.000000000000058620, -2.549999999999978506 ) ) ;
#16206 = ORIENTED_EDGE ( 'NONE', *, *, #4401, .T. ) ;
#16207 = DIRECTION ( 'NONE',  ( -0.000000000000000000, -0.000000000000000000, 1.000000000000000000 ) ) ;
#16208 = AXIS2_PLACEMENT_3D ( 'NONE', #20022, #9203, #19588 ) ;
#16209 = VECTOR ( 'NONE', #5638, 1000.000000000000000 ) ;
#16210 = CARTESIAN_POINT ( 'NONE',  ( 0.02893550784256185282, 0.6000000000000127454, -3.399425482353690242 ) ) ;
#16211 = LINE ( 'NONE', #3864, #12813 ) ;
#16212 = CARTESIAN_POINT ( 'NONE',  ( -7.271441198316233923, -13.72907106061213689, 8.039702399269760491 ) ) ;
#16213 = PLANE ( 'NONE',  #3204 ) ;
#16214 = CARTESIAN_POINT ( 'NONE',  ( -4.000000000000099476, -1.942223658245629148, -0.3516579909968203799 ) ) ;
#16215 = CARTESIAN_POINT ( 'NONE',  ( 4.104070371397483541, 2.023683613428375772, -3.505122836902498040 ) ) ;
#16216 = CARTESIAN_POINT ( 'NONE',  ( 0.000000000000000000, -3.031088913245536087, -1.750000000000001554 ) ) ;
#16217 = VECTOR ( 'NONE', #7817, 1000.000000000000000 ) ;
#16218 = DIRECTION ( 'NONE',  ( -2.220446049250313081E-16, 1.000000000000000000, -7.025792437124636392E-31 ) ) ;
#16219 = EDGE_LOOP ( 'NONE', ( #2414, #8409, #15170 ) ) ;
#16220 = SHAPE_DEFINITION_REPRESENTATION ( #20953, #17033 ) ;
#16221 = VECTOR ( 'NONE', #8565, 1000.000000000000000 ) ;
#16223 = ORIENTED_EDGE ( 'NONE', *, *, #204, .T. ) ;
#16222 = VERTEX_POINT ( 'NONE', #18084 ) ;
#16224 = TOROIDAL_SURFACE ( 'NONE', #1226, 1.300000000000000711, 0.5000000000000000000 ) ;
#16225 = AXIS2_PLACEMENT_3D ( 'NONE', #5968, #16410, #7380 ) ;
#16226 = PRODUCT_RELATED_PRODUCT_CATEGORY ( 'part', '', ( #838 ) ) ;
#16228 = EDGE_LOOP ( 'NONE', ( #12205, #22528, #21084, #8495 ) ) ;
#16227 = EDGE_LOOP ( 'NONE', ( #12060, #19753, #4529, #6707 ) ) ;
#16229 = CARTESIAN_POINT ( 'NONE',  ( -12.84999999999999964, -14.00000000000003020, 5.750000000000032863 ) ) ;
#16230 = CARTESIAN_POINT ( 'NONE',  ( 37.45482484129320966, 0.2122202663359486485, -2.956375721184415717 ) ) ;
#16231 = EDGE_CURVE ( 'NONE', #8601, #11150, #16963, .T. ) ;
#16232 = CARTESIAN_POINT ( 'NONE',  ( 8.719386969281462285, -12.50000000861905214, 6.820015264002557309 ) ) ;
#16233 = CIRCLE ( 'NONE', #12878, 6.500000000000075495 ) ;
#16234 = DIRECTION ( 'NONE',  ( 2.013525853228518840E-32, -6.902532920683810383E-31, 1.000000000000000000 ) ) ;
#16235 = DIRECTION ( 'NONE',  ( 2.891205793294682961E-15, 0.000000000000000000, 1.000000000000000000 ) ) ;
#16236 = DIRECTION ( 'NONE',  ( 3.032184104443271834E-30, 1.000000000000000000, 4.437342591868167759E-31 ) ) ;
#16237 = CARTESIAN_POINT ( 'NONE',  ( 0.000000000000000000, -1.750000000000001554, 0.000000000000000000 ) ) ;
#16238 = DIRECTION ( 'NONE',  ( 1.000000000000000000, 0.000000000000000000, 0.000000000000000000 ) ) ;
#16239 = ADVANCED_FACE ( 'NONE', ( #10670 ), #17853, .T. ) ;
#16240 = DIRECTION ( 'NONE',  ( 1.000000000000000000, -4.440892098500651800E-16, 0.000000000000000000 ) ) ;
#16241 = VECTOR ( 'NONE', #2045, 1000.000000000000000 ) ;
#16242 = LINE ( 'NONE', #10848, #4655 ) ;
#16243 = AXIS2_PLACEMENT_3D ( 'NONE', #13712, #2770, #13481 ) ;
#16244 = DIRECTION ( 'NONE',  ( 0.000000000000000000, 0.000000000000000000, -1.000000000000000000 ) ) ;
#16245 = EDGE_CURVE ( 'NONE', #17692, #1330, #22521, .T. ) ;
#16246 = VECTOR ( 'NONE', #16960, 1000.000000000000000 ) ;
#16247 = AXIS2_PLACEMENT_3D ( 'NONE', #16896, #8088, #2911 ) ;
#16248 = DIRECTION ( 'NONE',  ( 0.000000000000000000, 0.000000000000000000, 1.000000000000000000 ) ) ;
#16249 = DIRECTION ( 'NONE',  ( -0.000000000000000000, -0.000000000000000000, 1.000000000000000000 ) ) ;
#16250 = CARTESIAN_POINT ( 'NONE',  ( 7.756475484083233951, -0.06559517125032780782, 7.145789564688715956 ) ) ;
#16251 = ORIENTED_EDGE ( 'NONE', *, *, #12256, .T. ) ;
#16252 = SURFACE_STYLE_FILL_AREA ( #13087 ) ;
#16254 = ORIENTED_EDGE ( 'NONE', *, *, #5082, .T. ) ;
#16253 = ORIENTED_EDGE ( 'NONE', *, *, #18209, .F. ) ;
#16255 = B_SPLINE_CURVE_WITH_KNOTS ( 'NONE', 3,
 ( #17852, #5025, #17724, #14438 ),
 .UNSPECIFIED., .F., .F.,
 ( 4, 4 ),
 ( 2.380735702043570947E-07, 0.002775112046897009431 ),
 .UNSPECIFIED. ) ;
#16256 = VERTEX_POINT ( 'NONE', #21624 ) ;
#16257 = EDGE_CURVE ( 'NONE', #19696, #16772, #9604, .T. ) ;
#16258 = CIRCLE ( 'NONE', #8014, 2.500000000000015987 ) ;
#16260 = ORIENTED_EDGE ( 'NONE', *, *, #20460, .F. ) ;
#16259 = ORIENTED_EDGE ( 'NONE', *, *, #22021, .F. ) ;
#16261 = CIRCLE ( 'NONE', #7997, 7.500000000000001776 ) ;
#16262 = ORIENTED_EDGE ( 'NONE', *, *, #18294, .F. ) ;
#16263 = CONICAL_SURFACE ( 'NONE', #136, 2.060000000000002718, 0.9599310885968758145 ) ;
#16264 = DIRECTION ( 'NONE',  ( 0.5000000000000012212, -0.8660254037844379305, 6.428855108704667908E-16 ) ) ;
#16265 = CIRCLE ( 'NONE', #15146, 2.500000000000015543 ) ;
#16266 = ORIENTED_EDGE ( 'NONE', *, *, #22163, .F. ) ;
#16268 = EDGE_CURVE ( 'NONE', #22610, #18277, #12850, .T. ) ;
#16267 = AXIS2_PLACEMENT_3D ( 'NONE', #11318, #2619, #11214 ) ;
#16269 = EDGE_LOOP ( 'NONE', ( #3515, #16752, #12356, #20483 ) ) ;
#16270 = CARTESIAN_POINT ( 'NONE',  ( -6.000000000000074607, -5.300000000000023803, -7.500000000000034639 ) ) ;
#16271 = CARTESIAN_POINT ( 'NONE',  ( 0.000000000000000000, 0.000000000000000000, 0.000000000000000000 ) ) ;
#16272 = FACE_OUTER_BOUND ( 'NONE', #5265, .T. ) ;
#16273 = DIRECTION ( 'NONE',  ( -1.000000000000000000, 1.276756478318922922E-15, -1.333893503340766797E-15 ) ) ;
#16274 = EDGE_CURVE ( 'NONE', #20569, #21208, #18312, .T. ) ;
#16275 = DIRECTION ( 'NONE',  ( 0.6819983600625060260, 0.7313537016191635765, 6.106365041599011361E-16 ) ) ;
#16276 = CARTESIAN_POINT ( 'NONE',  ( -55.25320565519142946, -0.5000000000000281997, 8.000000000000076383 ) ) ;
#16277 = EDGE_CURVE ( 'NONE', #2970, #10913, #14724, .T. ) ;
#16278 = CARTESIAN_POINT ( 'NONE',  ( -3.453038570459517675, -2.625189405340010218, -3.535263753544271470 ) ) ;
#16279 = VECTOR ( 'NONE', #12671, 1000.000000000000000 ) ;
#16280 = SHAPE_REPRESENTATION ( 'Bolt', ( #22115 ), #22911 ) ;
#16281 = CIRCLE ( 'NONE', #9898, 0.2500000000000002220 ) ;
#16282 = FACE_OUTER_BOUND ( 'NONE', #15069, .T. ) ;
#16283 = AXIS2_PLACEMENT_3D ( 'NONE', #8218, #8329, #3039 ) ;
#16284 = DIRECTION ( 'NONE',  ( -1.000000000000000000, 1.389842848855773367E-62, -2.013525853228507892E-32 ) ) ;
#16285 = VECTOR ( 'NONE', #21151, 1000.000000000000000 ) ;
#16286 = VERTEX_POINT ( 'NONE', #13138 ) ;
#16287 = CIRCLE ( 'NONE', #21176, 0.4999999999999999445 ) ;
#16288 = SURFACE_SIDE_STYLE ('',( #13230 ) ) ;
#16289 = CARTESIAN_POINT ( 'NONE',  ( 0.000000000000000000, 0.000000000000000000, 0.000000000000000000 ) ) ;
#16290 = B_SPLINE_CURVE_WITH_KNOTS ( 'NONE', 3,
 ( #407, #5590, #14515, #14742, #9341, #11094, #3806, #16153, #18278, #3695 ),
 .UNSPECIFIED., .F., .F.,
 ( 4, 2, 2, 2, 4 ),
 ( 0.005493704601871788815, 0.006008885122700079531, 0.006524065643528370248, 0.007039246164356660965, 0.007554426685184951681 ),
 .UNSPECIFIED. ) ;
#16292 = VERTEX_POINT ( 'NONE', #20427 ) ;
#16291 = ORIENTED_EDGE ( 'NONE', *, *, #3338, .F. ) ;
#16293 = APPLICATION_CONTEXT ( 'automotive_design' ) ;
#16294 = EDGE_CURVE ( 'NONE', #22801, #9172, #2422, .T. ) ;
#16295 = ADVANCED_FACE ( 'NONE', ( #13243 ), #2653, .T. ) ;
#16296 = ADVANCED_FACE ( 'NONE', ( #11245 ), #668, .T. ) ;
#16297 = ADVANCED_FACE ( 'NONE', ( #13366 ), #5352, .T. ) ;
#16298 = EDGE_LOOP ( 'NONE', ( #9099, #16206, #8904, #17065 ) ) ;
#16299 = ORIENTED_EDGE ( 'NONE', *, *, #6870, .T. ) ;
#16300 = CARTESIAN_POINT ( 'NONE',  ( -42.54314575050785407, -4.000000000000034639, -7.500000000000007105 ) ) ;
#16301 = CIRCLE ( 'NONE', #19311, 2.500000000000000000 ) ;
#16302 = CIRCLE ( 'NONE', #1294, 0.5000000000000038858 ) ;
#16303 = DIRECTION ( 'NONE',  ( 6.106226635438366889E-16, -1.000000000000000000, 1.409037165336591006E-16 ) ) ;
#16304 = EDGE_CURVE ( 'NONE', #17692, #19662, #652, .T. ) ;
#16305 = TOROIDAL_SURFACE ( 'NONE', #6182, 6.500000000000000888, 0.5000000000000000000 ) ;
#16306 = CARTESIAN_POINT ( 'NONE',  ( 37.00000000000017053, 0.2500000000000002220, -10.43301270189217433 ) ) ;
#16307 = ADVANCED_FACE ( 'NONE', ( #2301, #8066, #4409 ), #5966, .F. ) ;
#16308 = DIRECTION ( 'NONE',  ( 1.000000000000000000, -4.440892098500654758E-16, 0.000000000000000000 ) ) ;
#16309 = DIRECTION ( 'NONE',  ( 2.220446049250313081E-16, -1.000000000000000000, 7.025792437124636392E-31 ) ) ;
#16310 = DIRECTION ( 'NONE',  ( -2.168404344971017743E-16, -1.000000000000000000, 6.982962677686261977E-15 ) ) ;
#16311 = DIRECTION ( 'NONE',  ( 0.000000000000000000, -1.000000000000000000, 0.000000000000000000 ) ) ;
#16312 = CARTESIAN_POINT ( 'NONE',  ( -7.268749084027565033, -2.258953384213796767, 7.689023314178085045 ) ) ;
#16313 = CARTESIAN_POINT ( 'NONE',  ( -3.999999999708153453, 38.99999999900385461, -18.50000000000000355 ) ) ;
#16314 = DIRECTION ( 'NONE',  ( -1.000000000000000000, -2.699383410053119644E-30, -3.330669073875432643E-16 ) ) ;
#16315 = DIRECTION ( 'NONE',  ( -3.885780586188016830E-16, -4.437342591868156373E-31, 1.000000000000000000 ) ) ;
#16316 = CARTESIAN_POINT ( 'NONE',  ( 37.48161866288228339, 0.1772999597157746965, -10.09721192197987705 ) ) ;
#16317 = CIRCLE ( 'NONE', #6191, 0.4999999999999995559 ) ;
#16318 = DIRECTION ( 'NONE',  ( 0.000000000000000000, 0.000000000000000000, -1.000000000000000000 ) ) ;
#16319 = AXIS2_PLACEMENT_3D ( 'NONE', #22392, #22617, #17194 ) ;
#16320 = PLANE ( 'NONE',  #8545 ) ;
#16321 = EDGE_LOOP ( 'NONE', ( #19345, #4020, #14194, #21244, #18620 ) ) ;
#16322 = ORIENTED_EDGE ( 'NONE', *, *, #5410, .T. ) ;
#16323 = FACE_OUTER_BOUND ( 'NONE', #16470, .T. ) ;
#16324 = FACE_OUTER_BOUND ( 'NONE', #20918, .T. ) ;
#16325 = ORIENTED_EDGE ( 'NONE', *, *, #2829, .F. ) ;
#16326 = DIRECTION ( 'NONE',  ( -1.000000000000000000, 0.000000000000000000, 0.000000000000000000 ) ) ;
#16327 = DIRECTION ( 'NONE',  ( 0.000000000000000000, 0.000000000000000000, 1.000000000000000000 ) ) ;
#16328 = CARTESIAN_POINT ( 'NONE',  ( 7.576750937466559144, -11.88724926130080206, 7.200086239788022091 ) ) ;
#16329 = CARTESIAN_POINT ( 'NONE',  ( 0.1217565302850851516, 2.351289329882099821, 2.927447417349521963 ) ) ;
#16330 = AXIS2_PLACEMENT_3D ( 'NONE', #707, #4101, #9290 ) ;
#16331 = VERTEX_POINT ( 'NONE', #22420 ) ;
#16332 = AXIS2_PLACEMENT_3D ( 'NONE', #1106, #2855, #6396 ) ;
#16333 = LINE ( 'NONE', #5763, #14048 ) ;
#16334 = CARTESIAN_POINT ( 'NONE',  ( -2.351786978051564260E-14, 0.3423821193870958401, 3.499999999999959588 ) ) ;
#16335 = CYLINDRICAL_SURFACE ( 'NONE', #1537, 5.999999999999998224 ) ;
#16336 = EDGE_CURVE ( 'NONE', #22532, #7024, #13018, .T. ) ;
#16337 = CARTESIAN_POINT ( 'NONE',  ( -6.960550854630949580, 36.00005224601497389, -18.51506780978411015 ) ) ;
#16338 = CARTESIAN_POINT ( 'NONE',  ( 8.496394830447192348, -13.96748264593550992, 6.998792816379823201 ) ) ;
#16339 = CARTESIAN_POINT ( 'NONE',  ( 3.999999999999955147, -2.309401076758532678, -3.433295621305388678 ) ) ;
#16340 = CARTESIAN_POINT ( 'NONE',  ( 4.180231891692622881, 4.134807952925586783, 0.02076457676759232637 ) ) ;
#16341 = B_SPLINE_CURVE_WITH_KNOTS ( 'NONE', 3,
 ( #3830, #10782, #12778, #18206, #21399, #21843, #10890, #14659, #5499, #16067, #20083, #9256, #11007, #5732, #8797, #19961 ),
 .UNSPECIFIED., .F., .F.,
 ( 4, 3, 3, 3, 3, 4 ),
 ( -2.111273352580643536E-06, 0.000000000000000000, 3.519286887793932848E-05, 7.191842652068034490E-05, 0.0001049868727093635162, 0.0001382836236822177726 ),
 .UNSPECIFIED. ) ;
#16342 = DIRECTION ( 'NONE',  ( 0.000000000000000000, 0.000000000000000000, 1.000000000000000000 ) ) ;
#16343 =( LENGTH_UNIT ( ) NAMED_UNIT ( * ) SI_UNIT ( .MILLI., .METRE. ) );
#16344 = CARTESIAN_POINT ( 'NONE',  ( -1.387778780781445676E-14, 2.000000000000001776, -1.500000000000001332 ) ) ;
#16345 = APPLICATION_PROTOCOL_DEFINITION ( 'draft international standard', 'automotive_design', 1998, #230 ) ;
#16346 = AXIS2_PLACEMENT_3D ( 'NONE', #8939, #11, #18001 ) ;
#16348 = ORIENTED_EDGE ( 'NONE', *, *, #7359, .T. ) ;
#16347 = ORIENTED_EDGE ( 'NONE', *, *, #15820, .F. ) ;
#16349 = ORIENTED_EDGE ( 'NONE', *, *, #22938, .T. ) ;
#16351 = VERTEX_POINT ( 'NONE', #11126 ) ;
#16350 = ORIENTED_EDGE ( 'NONE', *, *, #9806, .T. ) ;
#16352 = LINE ( 'NONE', #252, #8037 ) ;
#16353 = CARTESIAN_POINT ( 'NONE',  ( 37.46001462128806736, 0.1698019261547118741, -2.539985378711791419 ) ) ;
#16354 =( NAMED_UNIT ( * ) PLANE_ANGLE_UNIT ( ) SI_UNIT ( $, .RADIAN. ) );
#16355 = CARTESIAN_POINT ( 'NONE',  ( -3.999999999708139686, 35.99999999900384751, -18.99999999999998934 ) ) ;
#16356 = DIRECTION ( 'NONE',  ( -2.172745813409349776E-17, 1.000000000000000000, -1.309377075419428048E-16 ) ) ;
#16357 = DIRECTION ( 'NONE',  ( -1.135604581876758782E-15, -6.741645191078037727E-32, 1.000000000000000000 ) ) ;
#16358 = CARTESIAN_POINT ( 'NONE',  ( -3.999999999708152121, 38.75225147438559503, -15.99999999999998579 ) ) ;
#16359 =( LENGTH_UNIT ( ) NAMED_UNIT ( * ) SI_UNIT ( .MILLI., .METRE. ) );
#16360 = PLANE ( 'NONE',  #5777 ) ;
#16361 = DIRECTION ( 'NONE',  ( 0.7071067811865474617, -0.7071067811865474617, 0.000000000000000000 ) ) ;
#16362 = DIRECTION ( 'NONE',  ( -0.7313537016191742346, 0.6819983600624944797, 1.072890437865585765E-16 ) ) ;
#16363 = FACE_OUTER_BOUND ( 'NONE', #16227, .T. ) ;
#16364 = PLANE ( 'NONE',  #2513 ) ;
#16365 = TOROIDAL_SURFACE ( 'NONE', #17100, 5.750000000000000000, 0.5000000000000000000 ) ;
#16366 = CARTESIAN_POINT ( 'NONE',  ( 8.697224362267983011, -1.999999999999984457, 6.249999999999992006 ) ) ;
#16367 = DIRECTION ( 'NONE',  ( 1.000000000000000000, 4.440892098500626162E-16, -5.551115123125782702E-16 ) ) ;
#16368 = CARTESIAN_POINT ( 'NONE',  ( 7.651206356577009871, -0.8338323182648625931, 8.300907142094329672 ) ) ;
#16369 = VERTEX_POINT ( 'NONE', #20200 ) ;
#16370 = AXIS2_PLACEMENT_3D ( 'NONE', #13867, #22354, #17380 ) ;
#16371 = ADVANCED_FACE ( 'NONE', ( #558 ), #7720, .F. ) ;
#16373 = EDGE_LOOP ( 'NONE', ( #3056, #18775, #5012, #5960 ) ) ;
#16372 = ORIENTED_EDGE ( 'NONE', *, *, #761, .T. ) ;
#16374 = UNCERTAINTY_MEASURE_WITH_UNIT (LENGTH_MEASURE( 1.000000000000000082E-05 ), #6176, 'distance_accuracy_value', 'NONE');
#16375 = VERTEX_POINT ( 'NONE', #10410 ) ;
#16377 = VERTEX_POINT ( 'NONE', #9957 ) ;
#16376 = ORIENTED_EDGE ( 'NONE', *, *, #7761, .F. ) ;
#16378 = ORIENTED_EDGE ( 'NONE', *, *, #19165, .F. ) ;
#16379 = PLANE ( 'NONE',  #13258 ) ;
#16380 = ORIENTED_EDGE ( 'NONE', *, *, #2463, .T. ) ;
#16381 = ORIENTED_EDGE ( 'NONE', *, *, #21320, .F. ) ;
#16382 = CARTESIAN_POINT ( 'NONE',  ( 37.00000000000014211, 0.000000000000000000, -9.999999999999980460 ) ) ;
#16383 = DIRECTION ( 'NONE',  ( -1.000000000000000000, -1.479114197289388027E-30, 2.013525853228518840E-32 ) ) ;
#16384 = CARTESIAN_POINT ( 'NONE',  ( -87.15000000000063096, 5.607736497381665307E-14, -2.000000000000001332 ) ) ;
#16385 = DIRECTION ( 'NONE',  ( 9.121204216617949000E-31, 1.000000000000000000, -6.982962677686261977E-15 ) ) ;
#16386 = AXIS2_PLACEMENT_3D ( 'NONE', #8312, #17351, #15127 ) ;
#16387 = CARTESIAN_POINT ( 'NONE',  ( 4.175075985190096262, -2.060370777630243566, -3.568666869285537668 ) ) ;
#16388 = CARTESIAN_POINT ( 'NONE',  ( 3.806834918298672488, -3.031088913245592043, -1.750000000000008438 ) ) ;
#16389 = CARTESIAN_POINT ( 'NONE',  ( 54.42435809754106657, -4.000000000000003553, 6.000000000000136779 ) ) ;
#16390 = DIRECTION ( 'NONE',  ( -0.7453559924999295649, 0.000000000000000000, 0.6666666666666669627 ) ) ;
#16391 = EDGE_CURVE ( 'NONE', #2067, #10307, #13716, .T. ) ;
#16392 = CARTESIAN_POINT ( 'NONE',  ( -92.25000000000056843, -3.200000000000091216, -1.999999999999946265 ) ) ;
#16393 = CARTESIAN_POINT ( 'NONE',  ( 37.29045043747289156, 10.91119608832006449, -2.421762079371571730 ) ) ;
#16394 = ORIENTED_EDGE ( 'NONE', *, *, #2359, .T. ) ;
#16395 = EDGE_CURVE ( 'NONE', #22474, #19191, #13613, .T. ) ;
#16396 = DIRECTION ( 'NONE',  ( -1.000000000000000000, 1.276756478318922725E-15, -1.333893503340766402E-15 ) ) ;
#16398 = ORIENTED_EDGE ( 'NONE', *, *, #20199, .T. ) ;
#16397 = EDGE_LOOP ( 'NONE', ( #13128, #199 ) ) ;
#16399 = ORIENTED_EDGE ( 'NONE', *, *, #1522, .F. ) ;
#16400 =( GEOMETRIC_REPRESENTATION_CONTEXT ( 3 ) GLOBAL_UNCERTAINTY_ASSIGNED_CONTEXT ( ( #2493 ) ) GLOBAL_UNIT_ASSIGNED_CONTEXT ( ( #11423, #18608, #18716 ) ) REPRESENTATION_CONTEXT ( 'NONE', 'WORKASPACE' ) );
#16401 = EDGE_CURVE ( 'NONE', #5239, #12423, #12980, .T. ) ;
#16402 = ORIENTED_EDGE ( 'NONE', *, *, #20468, .T. ) ;
#16403 = EDGE_CURVE ( 'NONE', #22731, #14190, #361, .T. ) ;
#16404 = ORIENTED_EDGE ( 'NONE', *, *, #13783, .T. ) ;
#16405 = ORIENTED_EDGE ( 'NONE', *, *, #8339, .F. ) ;
#16406 = CYLINDRICAL_SURFACE ( 'NONE', #21200, 6.000000000000000000 ) ;
#16407 = TOROIDAL_SURFACE ( 'NONE', #11541, 0.7500000000000000000, 0.2500000000000000000 ) ;
#16408 = CARTESIAN_POINT ( 'NONE',  ( -7.499999999999992895, -8.000000000000044409, 6.250000000000005329 ) ) ;
#16409 = DIRECTION ( 'NONE',  ( 0.000000000000000000, 0.000000000000000000, 1.000000000000000000 ) ) ;
#16410 = DIRECTION ( 'NONE',  ( -0.7313537016191772322, -0.6819983600624914821, -3.241477906037841845E-14 ) ) ;
#16411 = CARTESIAN_POINT ( 'NONE',  ( -55.25320565519145788, 2.700000000000098321, 10.00000000000009237 ) ) ;
#16412 = AXIS2_PLACEMENT_3D ( 'NONE', #14348, #359, #8947 ) ;
#16413 = DIRECTION ( 'NONE',  ( 0.000000000000000000, -1.000000000000000000, 0.000000000000000000 ) ) ;
#16414 = DIRECTION ( 'NONE',  ( 0.7071067811865532349, 0.7071067811865419106, 0.000000000000000000 ) ) ;
#16415 = EDGE_CURVE ( 'NONE', #4164, #11689, #3100, .T. ) ;
#16416 = CIRCLE ( 'NONE', #19812, 2.500000000000002220 ) ;
#16417 = EDGE_CURVE ( 'NONE', #9134, #11001, #8426, .T. ) ;
#16418 = CARTESIAN_POINT ( 'NONE',  ( -7.613388670473280051, -13.11165441297978695, 8.423574099071748478 ) ) ;
#16419 = EDGE_CURVE ( 'NONE', #2526, #21123, #23019, .T. ) ;
#16420 = DIRECTION ( 'NONE',  ( 1.333893503340774882E-15, 2.778352770573747380E-17, 1.000000000000000000 ) ) ;
#16421 = DIRECTION ( 'NONE',  ( 1.000000000000000000, -1.550910762415513985E-16, -3.012982189080959477E-32 ) ) ;
#16422 = AXIS2_PLACEMENT_3D ( 'NONE', #21303, #5533, #7747 ) ;
#16423 = FACE_OUTER_BOUND ( 'NONE', #10079, .T. ) ;
#16424 = CIRCLE ( 'NONE', #11178, 0.4999999999999987232 ) ;
#16425 = DIRECTION ( 'NONE',  ( -1.000000000000000000, -1.479114197289397135E-31, -5.916456789157588541E-31 ) ) ;
#16426 = CARTESIAN_POINT ( 'NONE',  ( -89.70000000000059970, 0.5000000000000490719, 1.000000000000000888 ) ) ;
#16427 = ADVANCED_FACE ( 'NONE', ( #14058 ), #22772, .T. ) ;
#16428 = VECTOR ( 'NONE', #20529, 1000.000000000000000 ) ;
#16429 = ADVANCED_FACE ( 'NONE', ( #4532 ), #19352, .F. ) ;
#16430 = ORIENTED_EDGE ( 'NONE', *, *, #22175, .T. ) ;
#16431 = VECTOR ( 'NONE', #9382, 1000.000000000000000 ) ;
#16432 = EDGE_CURVE ( 'NONE', #11081, #16222, #3248, .T. ) ;
#16433 = AXIS2_PLACEMENT_3D ( 'NONE', #11807, #20765, #8406 ) ;
#16434 = CARTESIAN_POINT ( 'NONE',  ( -5.122455540400329355, 36.64919863988808402, -28.78988827279798812 ) ) ;
#16435 = DIRECTION ( 'NONE',  ( 0.6819983600624998088, -0.7313537016191693496, 0.000000000000000000 ) ) ;
#16436 = ORIENTED_EDGE ( 'NONE', *, *, #10707, .T. ) ;
#16437 = DIRECTION ( 'NONE',  ( -1.000000000000000000, -6.224605580259554159E-31, 2.887593071917436153E-31 ) ) ;
#16438 = LINE ( 'NONE', #21985, #18643 ) ;
#16439 = CARTESIAN_POINT ( 'NONE',  ( 7.862302507584137956, -11.95343515790908562, 6.866983975782649630 ) ) ;
#16440 = CARTESIAN_POINT ( 'NONE',  ( -6.938893903907228378E-14, 4.999999999999976907, -4.163336342344337027E-14 ) ) ;
#16441 = DIRECTION ( 'NONE',  ( 1.000000000000000000, 0.000000000000000000, 0.000000000000000000 ) ) ;
#16442 = VECTOR ( 'NONE', #2934, 1000.000000000000000 ) ;
#16443 = ORIENTED_EDGE ( 'NONE', *, *, #7822, .T. ) ;
#16444 = DIRECTION ( 'NONE',  ( 2.013525853228507892E-32, 6.902532920683810383E-31, -1.000000000000000000 ) ) ;
#16445 = AXIS2_PLACEMENT_3D ( 'NONE', #20240, #18934, #15620 ) ;
#16446 = DIRECTION ( 'NONE',  ( 9.121204216617949000E-31, 1.000000000000000000, -6.982962677686261977E-15 ) ) ;
#16447 = DIRECTION ( 'NONE',  ( 0.000000000000000000, 0.000000000000000000, 1.000000000000000000 ) ) ;
#16448 = CARTESIAN_POINT ( 'NONE',  ( 30.60000000000000142, 2.793567907494308344E-14, -2.055000000000020144 ) ) ;
#16449 = CARTESIAN_POINT ( 'NONE',  ( 7.132286784435703630, -13.57635026841701809, 8.470912490188352351 ) ) ;
#16450 = CARTESIAN_POINT ( 'NONE',  ( 8.216162181246719598, -1.557177370613327394, 7.299847320220724356 ) ) ;
#16451 = CARTESIAN_POINT ( 'NONE',  ( 4.158921614371308806, 1.986121848748776175, -3.559936047944516346 ) ) ;
#16452 = CARTESIAN_POINT ( 'NONE',  ( 54.42435809754109499, 0.4999999999999449329, 6.500000000000144773 ) ) ;
#16453 = CARTESIAN_POINT ( 'NONE',  ( 1.144235203016624736, 3.958177651039125777, -0.09382832055447234976 ) ) ;
#16454 = MECHANICAL_DESIGN_GEOMETRIC_PRESENTATION_REPRESENTATION (  '', ( #13466 ), #10475 ) ;
#16455 = CARTESIAN_POINT ( 'NONE',  ( 3.958484000406611525, -3.734437307742145329, -0.5317648453098834382 ) ) ;
#16456 = EDGE_CURVE ( 'NONE', #10432, #12501, #21884, .T. ) ;
#16457 = SHAPE_REPRESENTATION ( 'Bracket washer', ( #22115 ), #4465 ) ;
#16458 = AXIS2_PLACEMENT_3D ( 'NONE', #4566, #15389, #22577 ) ;
#16459 = PRODUCT_CONTEXT ( 'NONE', #10248, 'mechanical' ) ;
#16460 = CIRCLE ( 'NONE', #12317, 5.500000000000046185 ) ;
#16461 = TOROIDAL_SURFACE ( 'NONE', #13102, 3.500000000000000000, 0.5000000000000000000 ) ;
#16462 = ORIENTED_EDGE ( 'NONE', *, *, #896, .F. ) ;
#16463 = EDGE_CURVE ( 'NONE', #10215, #22156, #14927, .T. ) ;
#16464 = EDGE_CURVE ( 'NONE', #21027, #20045, #22542, .T. ) ;
#16465 = ORIENTED_EDGE ( 'NONE', *, *, #9406, .F. ) ;
#16467 = VERTEX_POINT ( 'NONE', #18892 ) ;
#16466 = ORIENTED_EDGE ( 'NONE', *, *, #9269, .F. ) ;
#16468 = DIRECTION ( 'NONE',  ( 1.000000000000000000, -4.190823558986610327E-31, 1.733449886265890494E-32 ) ) ;
#16469 = CARTESIAN_POINT ( 'NONE',  ( 37.51717533640922397, 0.02335407096342949698, -2.308399629903371331 ) ) ;
#16470 = EDGE_LOOP ( 'NONE', ( #7566, #17217, #12011, #18503 ) ) ;
#16471 = CARTESIAN_POINT ( 'NONE',  ( 4.151274195509691012, 4.079825909417423624, 3.209661024741434261E-15 ) ) ;
#16472 = CARTESIAN_POINT ( 'NONE',  ( 0.2499999999999932832, 2.775557561562891351E-14, -2.000000000000001776 ) ) ;
#16473 = CARTESIAN_POINT ( 'NONE',  ( 4.158413352280815545, -2.044871626972824430, 3.541821552872964851 ) ) ;
#16474 = DIRECTION ( 'NONE',  ( 1.000000000000000000, -1.550910762415513985E-16, -3.012982189080959477E-32 ) ) ;
#16475 = DIRECTION ( 'NONE',  ( 5.551115123125797493E-17, -2.869019762633797485E-16, -1.000000000000000000 ) ) ;
#16476 = AXIS2_PLACEMENT_3D ( 'NONE', #18781, #13724, #17114 ) ;
#16477 = CARTESIAN_POINT ( 'NONE',  ( 3.880358743661364240, 1.739972214219156044, -2.779021504384395325 ) ) ;
#16478 = CARTESIAN_POINT ( 'NONE',  ( 2.775557561562891351E-14, 0.5000000000000108802, -9.999999999999968026 ) ) ;
#16479 = CARTESIAN_POINT ( 'NONE',  ( -2.742413778650615086, -1.325747111984059590, -4.749999999999997335 ) ) ;
#16480 = DIRECTION ( 'NONE',  ( -0.000000000000000000, -1.000000000000000000, -0.000000000000000000 ) ) ;
#16481 = DIRECTION ( 'NONE',  ( 0.9706398123736330597, 1.076300044806638234E-16, 0.2405376366294442736 ) ) ;
#16482 = CARTESIAN_POINT ( 'NONE',  ( -6.000000000000019540, -4.800000000000006040, 7.500000000000062172 ) ) ;
#16483 = DIRECTION ( 'NONE',  ( 1.000000000000000000, -4.440892098500654758E-16, 0.000000000000000000 ) ) ;
#16484 = CARTESIAN_POINT ( 'NONE',  ( 7.604097569491915287, -0.4107518873690885752, 8.440516644273330371 ) ) ;
#16485 = ORIENTED_EDGE ( 'NONE', *, *, #16914, .T. ) ;
#16487 = EDGE_LOOP ( 'NONE', ( #7032, #8669, #19104, #16834 ) ) ;
#16486 = EDGE_LOOP ( 'NONE', ( #18800, #18395 ) ) ;
#16488 = ORIENTED_EDGE ( 'NONE', *, *, #19202, .F. ) ;
#16489 = CIRCLE ( 'NONE', #3376, 0.5000000000000029976 ) ;
#16490 = ORIENTED_EDGE ( 'NONE', *, *, #1852, .T. ) ;
#16492 = ORIENTED_EDGE ( 'NONE', *, *, #1693, .T. ) ;
#16491 = ORIENTED_EDGE ( 'NONE', *, *, #2522, .F. ) ;
#16493 = VERTEX_POINT ( 'NONE', #13600 ) ;
#16494 = DIRECTION ( 'NONE',  ( -1.445602896647339163E-16, 1.000000000000000000, -5.348730717595155471E-15 ) ) ;
#16495 = ORIENTED_EDGE ( 'NONE', *, *, #7259, .T. ) ;
#16496 = ORIENTED_EDGE ( 'NONE', *, *, #1771, .T. ) ;
#16497 = DIRECTION ( 'NONE',  ( 0.000000000000000000, -1.000000000000000000, 0.000000000000000000 ) ) ;
#16498 = CARTESIAN_POINT ( 'NONE',  ( 4.197393957002242715, -0.4069871074557576685, -3.503767560748912491 ) ) ;
#16499 = DIRECTION ( 'NONE',  ( 3.885780586188016830E-16, 4.437342591868156373E-31, -1.000000000000000000 ) ) ;
#16500 = AXIS2_PLACEMENT_3D ( 'NONE', #12468, #1542, #15999 ) ;
#16501 = DIRECTION ( 'NONE',  ( 1.000000000000000000, 3.254448077276381206E-32, 1.066788928082016908E-26 ) ) ;
#16502 = ADVANCED_FACE ( 'NONE', ( #11827 ), #20787, .F. ) ;
#16503 = CARTESIAN_POINT ( 'NONE',  ( 1.409656231407658705E-14, -22.49999999999996092, 7.882182279042401873 ) ) ;
#16504 = CYLINDRICAL_SURFACE ( 'NONE', #15344, 0.5000000000000037748 ) ;
#16505 = LINE ( 'NONE', #21945, #18938 ) ;
#16506 = PRESENTATION_STYLE_ASSIGNMENT (( #8888 ) ) ;
#16507 = LINE ( 'NONE', #11106, #9675 ) ;
#16508 = CARTESIAN_POINT ( 'NONE',  ( 37.86602540378468262, 11.00000000000000533, -2.133974596215522990 ) ) ;
#16509 = VERTEX_POINT ( 'NONE', #22658 ) ;
#16510 =( LENGTH_UNIT ( ) NAMED_UNIT ( * ) SI_UNIT ( .MILLI., .METRE. ) );
#16511 = DIRECTION ( 'NONE',  ( 2.220446049250313081E-16, -1.000000000000000000, 7.025792437124636392E-31 ) ) ;
#16512 = AXIS2_PLACEMENT_3D ( 'NONE', #21370, #19351, #71 ) ;
#16514 = VERTEX_POINT ( 'NONE', #3368 ) ;
#16513 = VERTEX_POINT ( 'NONE', #18063 ) ;
#16515 = EDGE_LOOP ( 'NONE', ( #10165, #19628, #12032, #19170 ) ) ;
#16516 = ORIENTED_EDGE ( 'NONE', *, *, #974, .F. ) ;
#16517 = VERTEX_POINT ( 'NONE', #12757 ) ;
#16518 = EDGE_CURVE ( 'NONE', #16375, #2238, #5374, .T. ) ;
#16519 = DIRECTION ( 'NONE',  ( -0.000000000000000000, 1.000000000000000000, -0.000000000000000000 ) ) ;
#16520 = CARTESIAN_POINT ( 'NONE',  ( 7.499999999999992895, -5.999999999999981348, 10.74999999999998224 ) ) ;
#16521 = CARTESIAN_POINT ( 'NONE',  ( -45.56568542494951402, -2.108831175456918228, -8.000000000000007105 ) ) ;
#16522 = EDGE_CURVE ( 'NONE', #13703, #4671, #288, .T. ) ;
#16523 = CARTESIAN_POINT ( 'NONE',  ( -2.000000000000119904, -3.464101615137792134, -1.040834085586084257E-14 ) ) ;
#16524 = CARTESIAN_POINT ( 'NONE',  ( 116.8476484622115805, -8.074585193523331483, -5.999999999999956479 ) ) ;
#16525 = CIRCLE ( 'NONE', #16899, 4.749999999999986677 ) ;
#16526 = CARTESIAN_POINT ( 'NONE',  ( 42.00000000000020606, 2.999999999999999112, -0.4999999999999449329 ) ) ;
#16527 = DIRECTION ( 'NONE',  ( -3.070652698126927723E-17, -1.000000000000000000, 4.167305704548413124E-17 ) ) ;
#16528 = CARTESIAN_POINT ( 'NONE',  ( -7.862302507584080224, -2.046564842090946801, 6.866983975782588345 ) ) ;
#16529 = DIRECTION ( 'NONE',  ( 1.000000000000000000, -1.276756478318922922E-15, 1.288690253661653294E-15 ) ) ;
#16530 = ADVANCED_FACE ( 'NONE', ( #1923 ), #9128, .T. ) ;
#16531 = ADVANCED_FACE ( 'NONE', ( #3809, #72 ), #19819, .F. ) ;
#16532 = DIRECTION ( 'NONE',  ( -1.000000000000000000, 5.551115122690166315E-17, 1.001543066815839268E-16 ) ) ;
#16533 = B_SPLINE_CURVE_WITH_KNOTS ( 'NONE', 3,
 ( #2864, #15440, #10502, #14151, #1685, #21458, #21342, #1793 ),
 .UNSPECIFIED., .F., .F.,
 ( 4, 2, 2, 4 ),
 ( 0.000000000000000000, 0.002450665683189821864, 0.003675998524784732796, 0.004901331366379644595 ),
 .UNSPECIFIED. ) ;
#16535 = EDGE_CURVE ( 'NONE', #21498, #9105, #19942, .T. ) ;
#16534 = CARTESIAN_POINT ( 'NONE',  ( 42.50000000000017764, 5.500000000000001776, 2.500000000000071498 ) ) ;
#16536 = FACE_OUTER_BOUND ( 'NONE', #20310, .T. ) ;
#16537 = CARTESIAN_POINT ( 'NONE',  ( 3.961545574370043177, 1.423222908133018549, -3.500000000000009326 ) ) ;
#16538 = AXIS2_PLACEMENT_3D ( 'NONE', #7891, #13422, #20603 ) ;
#16539 = ORIENTED_EDGE ( 'NONE', *, *, #2092, .T. ) ;
#16540 = CARTESIAN_POINT ( 'NONE',  ( -4.938244945965067245, 36.80742465210829550, -28.85443706880898418 ) ) ;
#16541 = EDGE_CURVE ( 'NONE', #17782, #21726, #6121, .T. ) ;
#16542 = EDGE_CURVE ( 'NONE', #8580, #4606, #17694, .T. ) ;
#16543 = LINE ( 'NONE', #9395, #22227 ) ;
#16544 =( BOUNDED_CURVE ( )  B_SPLINE_CURVE ( 3, ( #7249, #17704, #23012, #5000 ),
 .UNSPECIFIED., .F., .F. ) 
 B_SPLINE_CURVE_WITH_KNOTS ( ( 4, 4 ),
 ( 3.665191429188049632, 4.712388980384689674 ),
 .UNSPECIFIED. ) 
 CURVE ( )  GEOMETRIC_REPRESENTATION_ITEM ( )  RATIONAL_B_SPLINE_CURVE ( ( 1.000000000000000000, 0.9106836025229521070, 0.9106836025229521070, 1.000000000000000000 ) ) 
 REPRESENTATION_ITEM ( '' )  );
#16545 = ORIENTED_EDGE ( 'NONE', *, *, #19156, .T. ) ;
#16546 = CARTESIAN_POINT ( 'NONE',  ( 88.75737332930596324, -6.527605602963476805, 6.000000000000165201 ) ) ;
#16547 = CYLINDRICAL_SURFACE ( 'NONE', #8118, 0.4999999999999995559 ) ;
#16548 = CARTESIAN_POINT ( 'NONE',  ( 83.98338480886826574, -11.64708151429766403, -6.000000000000019540 ) ) ;
#16549 = EDGE_CURVE ( 'NONE', #11093, #6727, #14743, .T. ) ;
#16550 = CARTESIAN_POINT ( 'NONE',  ( 0.2175679805370102360, -1.691499766289419782, -3.500000000000035527 ) ) ;
#16551 = DIRECTION ( 'NONE',  ( 1.550910762415566494E-16, 1.000000000000000000, -8.135128085091684243E-31 ) ) ;
#16552 = DIRECTION ( 'NONE',  ( 1.454462294001240516E-30, 1.000000000000000000, 0.000000000000000000 ) ) ;
#16553 = CARTESIAN_POINT ( 'NONE',  ( 80.49335071782269324, -7.708908342713566064, -5.999999999999998224 ) ) ;
#16554 = CARTESIAN_POINT ( 'NONE',  ( 5.213674118231010013, -0.7499999999999520384, -2.999999999999995559 ) ) ;
#16555 = CARTESIAN_POINT ( 'NONE',  ( 8.115139842999440134, -13.89206392873120244, 7.423524081916067274 ) ) ;
#16556 = DIRECTION ( 'NONE',  ( -3.070652698126927723E-17, -1.000000000000000000, 4.167305704548413124E-17 ) ) ;
#16557 = ADVANCED_FACE ( 'NONE', ( #5359 ), #10754, .T. ) ;
#16558 = AXIS2_PLACEMENT_3D ( 'NONE', #13047, #9755, #939 ) ;
#16559 = STYLED_ITEM ( 'NONE', ( #3255 ), #20730 ) ;
#16560 = CARTESIAN_POINT ( 'NONE',  ( 6.999999999999978684, -10.98142396999974757, 8.916666666666712260 ) ) ;
#16561 = DIRECTION ( 'NONE',  ( 3.032184104443272185E-30, 1.000000000000000000, -7.395570986447005381E-32 ) ) ;
#16562 = LINE ( 'NONE', #4455, #19091 ) ;
#16563 = SHAPE_DEFINITION_REPRESENTATION ( #19646, #10586 ) ;
#16564 = ORIENTED_EDGE ( 'NONE', *, *, #6913, .F. ) ;
#16565 = ADVANCED_FACE ( 'NONE', ( #17941 ), #4592, .T. ) ;
#16566 = EDGE_CURVE ( 'NONE', #14654, #12162, #16607, .T. ) ;
#16568 = ORIENTED_EDGE ( 'NONE', *, *, #3492, .F. ) ;
#16567 = ORIENTED_EDGE ( 'NONE', *, *, #12388, .T. ) ;
#16569 = AXIS2_PLACEMENT_3D ( 'NONE', #15028, #13277, #20459 ) ;
#16570 = CARTESIAN_POINT ( 'NONE',  ( -8.697224362268011433, -12.00000000000004263, 6.250000000000019540 ) ) ;
#16571 = CYLINDRICAL_SURFACE ( 'NONE', #2450, 2.500000000000003997 ) ;
#16572 = CARTESIAN_POINT ( 'NONE',  ( 8.518530740350094277, -11.95646899714136957, 6.984205661426876155 ) ) ;
#16573 = ORIENTED_EDGE ( 'NONE', *, *, #12263, .T. ) ;
#16574 = CARTESIAN_POINT ( 'NONE',  ( 4.142654963991841299, 4.070796997468685063, 3.571802849091299743E-15 ) ) ;
#16575 = EDGE_CURVE ( 'NONE', #23124, #20629, #476, .T. ) ;
#16576 = CARTESIAN_POINT ( 'NONE',  ( -12.84999999999999964, -0.5000000000000038858, 5.750000000000018652 ) ) ;
#16577 = CARTESIAN_POINT ( 'NONE',  ( 0.6543461111163483279, 4.241015250120811153, -5.460849780464857695 ) ) ;
#16578 = CARTESIAN_POINT ( 'NONE',  ( 6.000000000291855429, -9.961476088449217059E-10, -5.999999999999998224 ) ) ;
#16579 = DIRECTION ( 'NONE',  ( 0.000000000000000000, 0.000000000000000000, 1.000000000000000000 ) ) ;
#16580 = DIRECTION ( 'NONE',  ( -1.000000000000000000, 4.795271322878693306E-14, -3.717264591378832268E-16 ) ) ;
#16581 = DIRECTION ( 'NONE',  ( -1.000000000000000000, -2.699383410053119644E-30, -3.330669073875432643E-16 ) ) ;
#16582 = SURFACE_STYLE_USAGE ( .BOTH. , #2599 ) ;
#16583 = CARTESIAN_POINT ( 'NONE',  ( -4.000000000000107470, 2.309401076758546445, -0.4999999999999865663 ) ) ;
#16584 = CARTESIAN_POINT ( 'NONE',  ( 0.2500000000000071609, 2.000000000000001776, 0.000000000000000000 ) ) ;
#16585 = EDGE_CURVE ( 'NONE', #11557, #16514, #7469, .T. ) ;
#16586 = CARTESIAN_POINT ( 'NONE',  ( 36.00000000029184832, -9.961476088449217059E-10, -5.999999999999998224 ) ) ;
#16587 = AXIS2_PLACEMENT_3D ( 'NONE', #7743, #7979, #11615 ) ;
#16588 = DIRECTION ( 'NONE',  ( -1.000000000000000000, -1.424116703980846297E-16, 1.095779650622964657E-32 ) ) ;
#16589 = CARTESIAN_POINT ( 'NONE',  ( 6.999999995223857852, -0.7826352830282113926, 9.233045673661260722 ) ) ;
#16590 = AXIS2_PLACEMENT_3D ( 'NONE', #559, #7493, #11350 ) ;
#16591 = VERTEX_POINT ( 'NONE', #5116 ) ;
#16592 = SHAPE_REPRESENTATION_RELATIONSHIP ( 'NONE' , 'NONE' ,  #11650, #1324 ) ;
#16594 = ORIENTED_EDGE ( 'NONE', *, *, #11099, .T. ) ;
#16593 = VERTEX_POINT ( 'NONE', #1708 ) ;
#16595 = UNCERTAINTY_MEASURE_WITH_UNIT (LENGTH_MEASURE( 1.000000000000000082E-05 ), #15433, 'distance_accuracy_value', 'NONE');
#16596 = ORIENTED_EDGE ( 'NONE', *, *, #20495, .T. ) ;
#16597 = ORIENTED_EDGE ( 'NONE', *, *, #3615, .F. ) ;
#16599 = ORIENTED_EDGE ( 'NONE', *, *, #8798, .T. ) ;
#16598 = ORIENTED_EDGE ( 'NONE', *, *, #16692, .T. ) ;
#16600 = AXIS2_PLACEMENT_3D ( 'NONE', #6743, #8509, #22751 ) ;
#16601 = VERTEX_POINT ( 'NONE', #8883 ) ;
#16602 = CARTESIAN_POINT ( 'NONE',  ( 86.02937988905583211, -9.453020409440155092, 6.000000000000165201 ) ) ;
#16603 = ORIENTED_EDGE ( 'NONE', *, *, #7395, .T. ) ;
#16604 = ORIENTED_EDGE ( 'NONE', *, *, #8640, .F. ) ;
#16605 = ADVANCED_FACE ( 'NONE', ( #7137 ), #21530, .T. ) ;
#16606 = DIRECTION ( 'NONE',  ( 2.013525853228507892E-32, 6.902532920683810383E-31, -1.000000000000000000 ) ) ;
#16607 = CIRCLE ( 'NONE', #9490, 3.499999999999999556 ) ;
#16608 = DIRECTION ( 'NONE',  ( 3.885780586188016830E-16, 4.437342591868156373E-31, -1.000000000000000000 ) ) ;
#16609 = CARTESIAN_POINT ( 'NONE',  ( 3.973110223767139626, -2.262956479381524922E-11, -3.565797985667441328 ) ) ;
#16610 = CIRCLE ( 'NONE', #12488, 2.100000000000011635 ) ;
#16611 = EDGE_CURVE ( 'NONE', #13097, #555, #22646, .T. ) ;
#16612 = AXIS2_PLACEMENT_3D ( 'NONE', #8282, #2632, #18630 ) ;
#16613 = CARTESIAN_POINT ( 'NONE',  ( -92.25000000000065370, 5.494493748869900097E-14, -2.000000000000001776 ) ) ;
#16614 = AXIS2_PLACEMENT_3D ( 'NONE', #573, #2213, #9167 ) ;
#16615 = DIRECTION ( 'NONE',  ( 0.000000000000000000, 0.000000000000000000, 1.000000000000000000 ) ) ;
#16616 = CARTESIAN_POINT ( 'NONE',  ( 4.071447262713891568, -4.041451884327432076, 1.040834085586084257E-14 ) ) ;
#16617 = CARTESIAN_POINT ( 'NONE',  ( 4.158806752148092478, -2.089318365061886951, 3.499999999999970246 ) ) ;
#16618 = FACE_OUTER_BOUND ( 'NONE', #3800, .T. ) ;
#16619 = EDGE_CURVE ( 'NONE', #19937, #19243, #2713, .T. ) ;
#16620 = CARTESIAN_POINT ( 'NONE',  ( 0.000000000000000000, 0.5000000000000108802, -10.86602540378443749 ) ) ;
#16621 = CARTESIAN_POINT ( 'NONE',  ( 37.00000000000030553, 10.74999999999999822, -2.566987298107756388 ) ) ;
#16622 = VERTEX_POINT ( 'NONE', #20289 ) ;
#16623 = UNCERTAINTY_MEASURE_WITH_UNIT (LENGTH_MEASURE( 1.000000000000000082E-05 ), #16715, 'distance_accuracy_value', 'NONE');
#16624 = CIRCLE ( 'NONE', #14394, 0.5000000000000033307 ) ;
#16625 = TOROIDAL_SURFACE ( 'NONE', #15927, 2.500000000000003997, 0.5000000000000000000 ) ;
#16626 = SURFACE_SIDE_STYLE ('',( #18639 ) ) ;
#16627 = FACE_OUTER_BOUND ( 'NONE', #13898, .T. ) ;
#16628 = AXIS2_PLACEMENT_3D ( 'NONE', #5899, #728, #16357 ) ;
#16630 = ORIENTED_EDGE ( 'NONE', *, *, #1636, .F. ) ;
#16629 = VERTEX_POINT ( 'NONE', #22277 ) ;
#16631 = MECHANICAL_DESIGN_GEOMETRIC_PRESENTATION_REPRESENTATION (  '', ( #10630 ), #4234 ) ;
#16632 = AXIS2_PLACEMENT_3D ( 'NONE', #21903, #7213, #2018 ) ;
#16633 = AXIS2_PLACEMENT_3D ( 'NONE', #9796, #14969, #18393 ) ;
#16634 = ORIENTED_EDGE ( 'NONE', *, *, #6783, .F. ) ;
#16635 = ORIENTED_EDGE ( 'NONE', *, *, #2050, .F. ) ;
#16636 = EDGE_LOOP ( 'NONE', ( #10691, #1801, #22966, #15067 ) ) ;
#16637 = DIRECTION ( 'NONE',  ( 5.551115123125782702E-16, 1.201780285297635172E-31, -1.000000000000000000 ) ) ;
#16638 = CARTESIAN_POINT ( 'NONE',  ( -2.742413778650712342, 1.325747111984031834, 4.749999999999999112 ) ) ;
#16639 = EDGE_LOOP ( 'NONE', ( #2850, #18526, #14651, #20966 ) ) ;
#16640 = DIRECTION ( 'NONE',  ( 2.013525853228507892E-32, 6.902532920683810383E-31, -1.000000000000000000 ) ) ;
#16641 = AXIS2_PLACEMENT_3D ( 'NONE', #21997, #5884, #5656 ) ;
#16642 = DIRECTION ( 'NONE',  ( -1.066786462891689527E-26, -6.656013887802287108E-31, -1.000000000000000000 ) ) ;
#16643 = CIRCLE ( 'NONE', #4633, 2.500000000000008882 ) ;
#16644 = DIRECTION ( 'NONE',  ( -0.7071067811865513475, 0.7071067811865437980, 2.580274238642642345E-14 ) ) ;
#16645 = CARTESIAN_POINT ( 'NONE',  ( -6.999999999999992006, -8.000000000000044409, 6.250000000000019540 ) ) ;
#16646 = AXIS2_PLACEMENT_3D ( 'NONE', #18342, #14577, #21764 ) ;
#16647 = CIRCLE ( 'NONE', #910, 4.750000000000000888 ) ;
#16648 = CARTESIAN_POINT ( 'NONE',  ( -7.670621117724550686, -11.48840066917088798, 8.215271161873666017 ) ) ;
#16649 = CIRCLE ( 'NONE', #21936, 7.000000000000075495 ) ;
#16650 = CIRCLE ( 'NONE', #17801, 0.5000000000000038858 ) ;
#16651 = CARTESIAN_POINT ( 'NONE',  ( -7.651206356577051615, -13.16616768173521557, 8.300907142094247959 ) ) ;
#16652 = CARTESIAN_POINT ( 'NONE',  ( -6.938893903907228378E-14, -4.618802153517121312, -5.000000000000011546 ) ) ;
#16653 = LINE ( 'NONE', #565, #5019 ) ;
#16654 = CARTESIAN_POINT ( 'NONE',  ( -5.261076337303340900, 1.454929939081866186, -0.3875484812920578226 ) ) ;
#16655 = PRODUCT_RELATED_PRODUCT_CATEGORY ( 'part', '', ( #21350 ) ) ;
#16656 = CARTESIAN_POINT ( 'NONE',  ( -50.65685424949273141, 7.200000000000025935, 8.000000000000076383 ) ) ;
#16657 = LINE ( 'NONE', #16767, #8931 ) ;
#16658 = ORIENTED_EDGE ( 'NONE', *, *, #3134, .F. ) ;
#16659 = EDGE_CURVE ( 'NONE', #9446, #18130, #12873, .T. ) ;
#16660 = VECTOR ( 'NONE', #16532, 1000.000000000000000 ) ;
#16661 = AXIS2_PLACEMENT_3D ( 'NONE', #20174, #8045, #14983 ) ;
#16662 = ORIENTED_EDGE ( 'NONE', *, *, #11974, .F. ) ;
#16663 = AXIS2_PLACEMENT_3D ( 'NONE', #10635, #3363, #15918 ) ;
#16664 = DIRECTION ( 'NONE',  ( 5.551115123561405253E-17, 1.000000000000000000, 2.256980353643891447E-27 ) ) ;
#16665 = CARTESIAN_POINT ( 'NONE',  ( -6.000000000000019540, -7.500000000000007105, 7.500000000000062172 ) ) ;
#16666 = ORIENTED_EDGE ( 'NONE', *, *, #22928, .T. ) ;
#16667 = CARTESIAN_POINT ( 'NONE',  ( -12.84999999999998721, -12.50000000000002842, 5.750000000000060396 ) ) ;
#16668 = CARTESIAN_POINT ( 'NONE',  ( 5.550000000291854363, 42.99999999900385461, -26.00000000000000000 ) ) ;
#16669 = DIRECTION ( 'NONE',  ( 1.000000000000000000, 1.065615849528602702E-14, 0.000000000000000000 ) ) ;
#16670 = FACE_OUTER_BOUND ( 'NONE', #9335, .T. ) ;
#16671 = CYLINDRICAL_SURFACE ( 'NONE', #21198, 0.5000000000000025535 ) ;
#16672 = DIRECTION ( 'NONE',  ( 3.254448077146059901E-32, 1.000000000000000000, 6.409494854920712161E-31 ) ) ;
#16673 = VERTEX_POINT ( 'NONE', #410 ) ;
#16674 = CARTESIAN_POINT ( 'NONE',  ( 12.84999999999999964, -2.000000000000005329, -5.749999999999991118 ) ) ;
#16675 = FACE_OUTER_BOUND ( 'NONE', #22263, .T. ) ;
#16676 = CARTESIAN_POINT ( 'NONE',  ( 7.029812747553616958, -13.37717092480913372, 8.933015330925693220 ) ) ;
#16677 = CIRCLE ( 'NONE', #23092, 4.000000000000000888 ) ;
#16678 = CARTESIAN_POINT ( 'NONE',  ( 0.3126073911696447549, -4.041451884327383226, 0.000000000000000000 ) ) ;
#16679 = AXIS2_PLACEMENT_3D ( 'NONE', #7080, #5538, #18115 ) ;
#16680 = CARTESIAN_POINT ( 'NONE',  ( 83.98338480886830837, -11.64708151429766403, 6.000000000000136779 ) ) ;
#16681 = LINE ( 'NONE', #590, #13840 ) ;
#16682 =( GEOMETRIC_REPRESENTATION_CONTEXT ( 3 ) GLOBAL_UNCERTAINTY_ASSIGNED_CONTEXT ( ( #5818 ) ) GLOBAL_UNIT_ASSIGNED_CONTEXT ( ( #4146, #22618, #9800 ) ) REPRESENTATION_CONTEXT ( 'NONE', 'WORKASPACE' ) );
#16683 = FACE_OUTER_BOUND ( 'NONE', #10934, .T. ) ;
#16684 = EDGE_CURVE ( 'NONE', #14824, #17188, #14748, .T. ) ;
#16685 = CARTESIAN_POINT ( 'NONE',  ( -2.700000000000063238, -2.000000000000043521, 8.000000000000076383 ) ) ;
#16686 = ADVANCED_FACE ( 'NONE', ( #644 ), #14868, .F. ) ;
#16687 = ITEM_DEFINED_TRANSFORMATION ( 'NONE', 'NONE', #18399,  #22115 ) ;
#16688 = ORIENTED_EDGE ( 'NONE', *, *, #10553, .T. ) ;
#16691 = ORIENTED_EDGE ( 'NONE', *, *, #6611, .F. ) ;
#16690 = EDGE_CURVE ( 'NONE', #4569, #11578, #531, .T. ) ;
#16689 = VERTEX_POINT ( 'NONE', #871 ) ;
#16692 = EDGE_CURVE ( 'NONE', #2652, #4603, #5740, .T. ) ;
#16693 = CARTESIAN_POINT ( 'NONE',  ( 88.75737332930596324, -13.02760560296348302, -6.499999999999964473 ) ) ;
#16694 = CARTESIAN_POINT ( 'NONE',  ( 37.73505106183394986, 7.718611010957700083E-12, -2.264948938170268544 ) ) ;
#16695 = CARTESIAN_POINT ( 'NONE',  ( 3.000000000291852764, 42.99999999900385461, 0.000000000000000000 ) ) ;
#16696 = ORIENTED_EDGE ( 'NONE', *, *, #19433, .T. ) ;
#16697 = CARTESIAN_POINT ( 'NONE',  ( -43.46238456605047418, 4.919238815542508192, 8.000000000000035527 ) ) ;
#16698 = CARTESIAN_POINT ( 'NONE',  ( -45.91923881554273379, -2.462384566050232593, 7.500000000000034639 ) ) ;
#16699 = CARTESIAN_POINT ( 'NONE',  ( 4.330127018922110160, 4.689110867544560080, 7.499999999999985789 ) ) ;
#16700 = DIRECTION ( 'NONE',  ( -4.190823558986625216E-31, 1.000000000000000000, -4.190823558986625216E-31 ) ) ;
#16701 = DIRECTION ( 'NONE',  ( 0.000000000000000000, 1.000000000000000000, 0.000000000000000000 ) ) ;
#16702 = DIRECTION ( 'NONE',  ( -1.066194817212773768E-26, 0.000000000000000000, -1.000000000000000000 ) ) ;
#16703 = DIRECTION ( 'NONE',  ( -0.000000000000000000, -0.000000000000000000, 1.000000000000000000 ) ) ;
#16704 = CARTESIAN_POINT ( 'NONE',  ( 115.1426525620552468, -6.246200939475476943, -6.499999999999950262 ) ) ;
#16705 = PLANE ( 'NONE',  #4171 ) ;
#16706 = EDGE_CURVE ( 'NONE', #7197, #18871, #14376, .T. ) ;
#16707 = EDGE_CURVE ( 'NONE', #371, #3970, #4984, .T. ) ;
#16708 = VECTOR ( 'NONE', #17496, 1000.000000000000000 ) ;
#16709 = EDGE_CURVE ( 'NONE', #11150, #21697, #7254, .T. ) ;
#16710 = LINE ( 'NONE', #7250, #21211 ) ;
#16711 = DIRECTION ( 'NONE',  ( -1.000000000000000000, 4.190823558986610327E-31, -1.733449886265890494E-32 ) ) ;
#16712 = CARTESIAN_POINT ( 'NONE',  ( 4.050880675075942960, 1.379097446046193998, 3.567934390854428095 ) ) ;
#16713 = CARTESIAN_POINT ( 'NONE',  ( 6.000000000291855429, -9.961476088449217059E-10, -39.00000000000000000 ) ) ;
#16714 = ORIENTED_EDGE ( 'NONE', *, *, #17872, .T. ) ;
#16715 =( LENGTH_UNIT ( ) NAMED_UNIT ( * ) SI_UNIT ( .MILLI., .METRE. ) );
#16717 = EDGE_LOOP ( 'NONE', ( #20390, #15604, #21556, #14733 ) ) ;
#16716 = VERTEX_POINT ( 'NONE', #4267 ) ;
#16718 = EDGE_CURVE ( 'NONE', #11081, #14890, #7700, .T. ) ;
#16719 = VERTEX_POINT ( 'NONE', #22047 ) ;
#16720 = VERTEX_POINT ( 'NONE', #2280 ) ;
#16723 = ORIENTED_EDGE ( 'NONE', *, *, #3761, .F. ) ;
#16722 = ADVANCED_FACE ( 'NONE', ( #18629 ), #14639, .F. ) ;
#16721 = ORIENTED_EDGE ( 'NONE', *, *, #4653, .F. ) ;
#16724 = AXIS2_PLACEMENT_3D ( 'NONE', #23163, #840, #213 ) ;
#16725 = ORIENTED_EDGE ( 'NONE', *, *, #18294, .T. ) ;
#16726 = DIRECTION ( 'NONE',  ( 1.454462294001240516E-30, 1.000000000000000000, 0.000000000000000000 ) ) ;
#16727 = EDGE_CURVE ( 'NONE', #15429, #1571, #115, .T. ) ;
#16728 = ORIENTED_EDGE ( 'NONE', *, *, #22846, .T. ) ;
#16729 = VERTEX_POINT ( 'NONE', #2398 ) ;
#16730 = CYLINDRICAL_SURFACE ( 'NONE', #14458, 0.5000000000000022204 ) ;
#16731 = ADVANCED_FACE ( 'NONE', ( #12992 ), #8188, .T. ) ;
#16732 = LINE ( 'NONE', #2626, #6277 ) ;
#16733 = CARTESIAN_POINT ( 'NONE',  ( -95.20000000000065654, -2.700000000000119194, -2.000000000000001776 ) ) ;
#16734 = CARTESIAN_POINT ( 'NONE',  ( -65.00000000000044054, -2.700000000000084110, 2.999999999999947153 ) ) ;
#16735 = CARTESIAN_POINT ( 'NONE',  ( -7.725871784772690098, -1.814340584915019372, 8.100883686805044448 ) ) ;
#16736 = CIRCLE ( 'NONE', #18355, 0.2500000000000002220 ) ;
#16737 = CARTESIAN_POINT ( 'NONE',  ( 10.49999999999999467, -13.50000000000000888, 9.250000000000063949 ) ) ;
#16738 = DIRECTION ( 'NONE',  ( 2.775557561562883031E-17, 1.309377075419427801E-16, 1.000000000000000000 ) ) ;
#16739 = DIRECTION ( 'NONE',  ( -1.000000000000000000, -0.000000000000000000, 0.000000000000000000 ) ) ;
#16740 = DIRECTION ( 'NONE',  ( -1.550910762415566494E-16, -1.000000000000000000, 8.135128085091684243E-31 ) ) ;
#16741 = CIRCLE ( 'NONE', #5135, 5.500000000000000000 ) ;
#16742 = CARTESIAN_POINT ( 'NONE',  ( 0.1397371499203269585, 1.362866705341221785, -3.500000000000035083 ) ) ;
#16743 = DIRECTION ( 'NONE',  ( 0.000000000000000000, 0.000000000000000000, 1.000000000000000000 ) ) ;
#16744 = VERTEX_POINT ( 'NONE', #21095 ) ;
#16746 = ORIENTED_EDGE ( 'NONE', *, *, #17269, .F. ) ;
#16745 = EDGE_LOOP ( 'NONE', ( #5060, #6417, #4391, #22303 ) ) ;
#16747 = ORIENTED_EDGE ( 'NONE', *, *, #13692, .T. ) ;
#16748 = AXIS2_PLACEMENT_3D ( 'NONE', #18676, #9170, #16327 ) ;
#16749 = ORIENTED_EDGE ( 'NONE', *, *, #11324, .T. ) ;
#16750 = EDGE_CURVE ( 'NONE', #10858, #16514, #3118, .T. ) ;
#16751 = CIRCLE ( 'NONE', #3267, 2.500000000000008882 ) ;
#16752 = ORIENTED_EDGE ( 'NONE', *, *, #10957, .F. ) ;
#16753 = CARTESIAN_POINT ( 'NONE',  ( -53.99613665484947944, -1.040834085586084257E-13, -13.19342998475045370 ) ) ;
#16754 = LINE ( 'NONE', #666, #14400 ) ;
#16755 = VERTEX_POINT ( 'NONE', #13911 ) ;
#16756 = DIRECTION ( 'NONE',  ( 3.032184104443272185E-30, 1.000000000000000000, -7.395570986447005381E-32 ) ) ;
#16757 = LINE ( 'NONE', #14778, #21887 ) ;
#16758 = FACE_OUTER_BOUND ( 'NONE', #3353, .T. ) ;
#16759 = DIRECTION ( 'NONE',  ( 2.775557561562883647E-17, -3.652049423109057473E-16, 1.000000000000000000 ) ) ;
#16760 = CARTESIAN_POINT ( 'NONE',  ( -8.719386969281412547, -12.50000000861904859, 6.820015264002559974 ) ) ;
#16761 = DIRECTION ( 'NONE',  ( 2.172745813409349776E-17, -1.000000000000000000, 1.309377075419428048E-16 ) ) ;
#16762 = CARTESIAN_POINT ( 'NONE',  ( -4.857225732735059864E-14, 4.999999999999976907, -7.500000000000003553 ) ) ;
#16763 = DIRECTION ( 'NONE',  ( 0.000000000000000000, -6.938893903907237844E-15, -1.000000000000000000 ) ) ;
#16764 = CARTESIAN_POINT ( 'NONE',  ( 2.074729277268261285E-14, 10.00000000000000533, -2.500000000000006661 ) ) ;
#16765 = VECTOR ( 'NONE', #17560, 1000.000000000000114 ) ;
#16766 = DIRECTION ( 'NONE',  ( 0.000000000000000000, 3.382522293539643228E-32, 1.000000000000000000 ) ) ;
#16767 = CARTESIAN_POINT ( 'NONE',  ( 8.660254037844344666, -2.775557561562891351E-14, 2.081668171172168513E-14 ) ) ;
#16769 = ORIENTED_EDGE ( 'NONE', *, *, #13900, .T. ) ;
#16768 = CIRCLE ( 'NONE', #5137, 0.4999999999999990563 ) ;
#16770 = EDGE_LOOP ( 'NONE', ( #1409, #4028, #2724, #11599 ) ) ;
#16771 = ORIENTED_EDGE ( 'NONE', *, *, #14443, .F. ) ;
#16772 = VERTEX_POINT ( 'NONE', #3220 ) ;
#16773 = DIRECTION ( 'NONE',  ( 0.000000000000000000, -4.190823558986610327E-31, 1.000000000000000000 ) ) ;
#16774 = CARTESIAN_POINT ( 'NONE',  ( -4.000000000000003553, 0.000000000000000000, -5.600000000000000533 ) ) ;
#16775 = VERTEX_POINT ( 'NONE', #17311 ) ;
#16776 = CARTESIAN_POINT ( 'NONE',  ( -4.550510256924974684, 36.49999999900384751, -19.00000000000000355 ) ) ;
#16777 = CARTESIAN_POINT ( 'NONE',  ( -4.690415759823415520, -0.7499999999999382716, -1.500000000000001332 ) ) ;
#16778 = CIRCLE ( 'NONE', #17548, 0.4999999999999995559 ) ;
#16779 = FACE_OUTER_BOUND ( 'NONE', #1269, .T. ) ;
#16780 = ORIENTED_EDGE ( 'NONE', *, *, #17014, .F. ) ;
#16781 = DIRECTION ( 'NONE',  ( 3.759415251443883509E-31, -0.8660254037844378194, 0.5000000000000014433 ) ) ;
#16782 = DIRECTION ( 'NONE',  ( 1.000000000000000000, 0.000000000000000000, 0.000000000000000000 ) ) ;
#16783 = FACE_OUTER_BOUND ( 'NONE', #15461, .T. ) ;
#16784 = DIRECTION ( 'NONE',  ( -4.190823558986625216E-31, 1.000000000000000000, -4.190823558986625216E-31 ) ) ;
#16785 = EDGE_CURVE ( 'NONE', #235, #10831, #4962, .T. ) ;
#16786 = CIRCLE ( 'NONE', #4386, 11.16066016895667268 ) ;
#16787 = DIRECTION ( 'NONE',  ( 1.000000000000000000, 0.000000000000000000, 0.000000000000000000 ) ) ;
#16788 = CARTESIAN_POINT ( 'NONE',  ( 3.961551342854520819, 3.742715940867734847, -0.5174258321191672616 ) ) ;
#16789 = CYLINDRICAL_SURFACE ( 'NONE', #4443, 4.000000000000045297 ) ;
#16791 = AXIS2_PLACEMENT_3D ( 'NONE', #12877, #9236, #20061 ) ;
#16790 = CARTESIAN_POINT ( 'NONE',  ( -12.85000000000002807, -12.50000000000002842, 6.250000000000061284 ) ) ;
#16792 = LINE ( 'NONE', #713, #11945 ) ;
#16793 = CIRCLE ( 'NONE', #7058, 2.500000000000002220 ) ;
#16794 = ORIENTED_EDGE ( 'NONE', *, *, #7539, .T. ) ;
#16795 = VECTOR ( 'NONE', #16249, 1000.000000000000000 ) ;
#16796 = CONTEXT_DEPENDENT_SHAPE_REPRESENTATION ( #13009, #17561 ) ;
#16797 = ORIENTED_EDGE ( 'NONE', *, *, #8765, .T. ) ;
#16798 = AXIS2_PLACEMENT_3D ( 'NONE', #8828, #17640, #3749 ) ;
#16799 = AXIS2_PLACEMENT_3D ( 'NONE', #3682, #9326, #1798 ) ;
#16801 = ORIENTED_EDGE ( 'NONE', *, *, #20091, .F. ) ;
#16800 = EDGE_LOOP ( 'NONE', ( #9221, #10882, #20972, #8148 ) ) ;
#16802 = FACE_OUTER_BOUND ( 'NONE', #5987, .T. ) ;
#16803 = CARTESIAN_POINT ( 'NONE',  ( 12.84999999999998721, -12.50000000000002842, 6.250000000000074607 ) ) ;
#16804 = FILL_AREA_STYLE_COLOUR ( '', #20820 ) ;
#16805 = VERTEX_POINT ( 'NONE', #2859 ) ;
#16806 = LINE ( 'NONE', #22243, #10478 ) ;
#16807 = CARTESIAN_POINT ( 'NONE',  ( 3.674234614174737068, -0.7499999999999451550, -3.000000000000002665 ) ) ;
#16808 = DIRECTION ( 'NONE',  ( 1.000000000000000000, -1.276756478318923119E-15, 1.387778780781436998E-15 ) ) ;
#16809 = CIRCLE ( 'NONE', #3672, 6.500000000000075495 ) ;
#16810 = EDGE_CURVE ( 'NONE', #10973, #19482, #15323, .T. ) ;
#16811 = CARTESIAN_POINT ( 'NONE',  ( -4.614318463248863189, 37.16513102274243607, -16.05878810958467895 ) ) ;
#16812 = SURFACE_STYLE_FILL_AREA ( #9316 ) ;
#16813 = FACE_OUTER_BOUND ( 'NONE', #17506, .T. ) ;
#16814 = DIRECTION ( 'NONE',  ( 0.000000000000000000, 0.000000000000000000, 1.000000000000000000 ) ) ;
#16815 = DIRECTION ( 'NONE',  ( -0.000000000000000000, -0.000000000000000000, 1.000000000000000000 ) ) ;
#16816 = DIRECTION ( 'NONE',  ( -5.551115123125733398E-17, 0.000000000000000000, 1.000000000000000000 ) ) ;
#16817 = CIRCLE ( 'NONE', #21366, 6.000000000000047073 ) ;
#16818 = EDGE_CURVE ( 'NONE', #22996, #2097, #15101, .T. ) ;
#16819 = CARTESIAN_POINT ( 'NONE',  ( 29.00000000029184832, 16.99999999900385461, -19.00000000000000355 ) ) ;
#16820 = AXIS2_PLACEMENT_3D ( 'NONE', #6004, #2575, #7642 ) ;
#16821 = FACE_OUTER_BOUND ( 'NONE', #2415, .T. ) ;
#16822 = CIRCLE ( 'NONE', #5593, 3.999999999999999112 ) ;
#16823 = ADVANCED_FACE ( 'NONE', ( #22513 ), #17434, .T. ) ;
#16824 = DIRECTION ( 'NONE',  ( 1.000000000000000000, 1.479114197289388027E-30, -2.013525853228518840E-32 ) ) ;
#16825 = CARTESIAN_POINT ( 'NONE',  ( 6.000000000291855429, 2.999999999003851503, 0.000000000000000000 ) ) ;
#16826 = EDGE_CURVE ( 'NONE', #13088, #6327, #6858, .T. ) ;
#16827 = ORIENTED_EDGE ( 'NONE', *, *, #11264, .F. ) ;
#16829 = VERTEX_POINT ( 'NONE', #6401 ) ;
#16828 = EDGE_LOOP ( 'NONE', ( #19239, #2669, #7799, #15882 ) ) ;
#16830 = UNCERTAINTY_MEASURE_WITH_UNIT (LENGTH_MEASURE( 1.000000000000000082E-05 ), #5192, 'distance_accuracy_value', 'NONE');
#16831 = AXIS2_PLACEMENT_3D ( 'NONE', #22602, #11538, #9667 ) ;
#16832 = EDGE_LOOP ( 'NONE', ( #9215, #18877, #20329, #11894 ) ) ;
#16833 = ORIENTED_EDGE ( 'NONE', *, *, #20908, .F. ) ;
#16835 = VERTEX_POINT ( 'NONE', #1220 ) ;
#16834 = ORIENTED_EDGE ( 'NONE', *, *, #13361, .F. ) ;
#16836 = EDGE_LOOP ( 'NONE', ( #7287, #16495 ) ) ;
#16837 = DIRECTION ( 'NONE',  ( -3.241725282392603095E-30, -1.000000000000000000, 2.218671295934100958E-31 ) ) ;
#16838 = CARTESIAN_POINT ( 'NONE',  ( 2.918498775983380256E-10, -9.961476088449217059E-10, -5.999999999999998224 ) ) ;
#16839 = ORIENTED_EDGE ( 'NONE', *, *, #10639, .T. ) ;
#16840 = EDGE_CURVE ( 'NONE', #12651, #10401, #13796, .T. ) ;
#16841 = CARTESIAN_POINT ( 'NONE',  ( 4.071447262713891568, 4.041451884327377009, -2.081668171172168513E-14 ) ) ;
#16842 = CIRCLE ( 'NONE', #12328, 4.500000000000000888 ) ;
#16843 = EDGE_CURVE ( 'NONE', #18558, #9711, #9020, .T. ) ;
#16844 = AXIS2_PLACEMENT_3D ( 'NONE', #17235, #1144, #13606 ) ;
#16845 = B_SPLINE_CURVE_WITH_KNOTS ( 'NONE', 3,
 ( #19385, #5511, #12673, #19859 ),
 .UNSPECIFIED., .F., .F.,
 ( 4, 4 ),
 ( 2.309401076552564490E-07, 0.004330357959029877170 ),
 .UNSPECIFIED. ) ;
#16846 = CIRCLE ( 'NONE', #4833, 1.000000000000000000 ) ;
#16847 = CARTESIAN_POINT ( 'NONE',  ( -56.91911807125110556, 1.387778780781445676E-14, -8.333333333333358794 ) ) ;
#16848 = DIRECTION ( 'NONE',  ( -2.013525853228507892E-32, -6.902532920683810383E-31, 1.000000000000000000 ) ) ;
#16849 = CARTESIAN_POINT ( 'NONE',  ( 3.012908790756472548E-16, 1.291058893185205491E-15, 4.499999999999988454 ) ) ;
#16850 = DIRECTION ( 'NONE',  ( -1.000000000000000000, -1.479114197289397135E-31, -5.916456789157588541E-31 ) ) ;
#16851 = FACE_OUTER_BOUND ( 'NONE', #1541, .T. ) ;
#16852 = CARTESIAN_POINT ( 'NONE',  ( 6.999999991928306464, -2.825498329575450551, 8.700799235122079978 ) ) ;
#16853 = CARTESIAN_POINT ( 'NONE',  ( -4.000000000000103917, 2.309401076758544225, -3.504269196027523403 ) ) ;
#16854 = EDGE_CURVE ( 'NONE', #7230, #7125, #12508, .T. ) ;
#16855 = SURFACE_STYLE_USAGE ( .BOTH. , #14984 ) ;
#16856 = COLOUR_RGB ( '', 0.66274510, 0.83137255, 0.94901961) ;
#16857 = CARTESIAN_POINT ( 'NONE',  ( -57.28378781035996070, -3.200000000000108979, 8.541666666666781538 ) ) ;
#16858 = EDGE_CURVE ( 'NONE', #23243, #14397, #5941, .T. ) ;
#16859 = PLANE ( 'NONE',  #12331 ) ;
#16860 = CARTESIAN_POINT ( 'NONE',  ( 5.384454397937147974, -6.874637034779069804E-15, -4.999999999999993783 ) ) ;
#16861 = CARTESIAN_POINT ( 'NONE',  ( 0.000000000000000000, 0.000000000000000000, 3.469446951953614189E-15 ) ) ;
#16862 = ADVANCED_FACE ( 'NONE', ( #6854 ), #16993, .T. ) ;
#16863 = EDGE_LOOP ( 'NONE', ( #14391, #20072, #892, #2030 ) ) ;
#16864 = AXIS2_PLACEMENT_3D ( 'NONE', #8974, #19792, #10607 ) ;
#16866 = ORIENTED_EDGE ( 'NONE', *, *, #2786, .T. ) ;
#16865 = VERTEX_POINT ( 'NONE', #19910 ) ;
#16867 = VERTEX_POINT ( 'NONE', #18031 ) ;
#16868 = EDGE_LOOP ( 'NONE', ( #17274, #9396, #2277, #16251 ) ) ;
#16869 = ORIENTED_EDGE ( 'NONE', *, *, #21629, .T. ) ;
#16870 = MECHANICAL_DESIGN_GEOMETRIC_PRESENTATION_REPRESENTATION (  '', ( #7136 ), #4100 ) ;
#16871 = ORIENTED_EDGE ( 'NONE', *, *, #2239, .T. ) ;
#16872 = FACE_OUTER_BOUND ( 'NONE', #15649, .T. ) ;
#16873 = EDGE_CURVE ( 'NONE', #9093, #4926, #12482, .T. ) ;
#16874 = B_SPLINE_CURVE_WITH_KNOTS ( 'NONE', 3,
 ( #2250, #16577, #14835, #2835 ),
 .UNSPECIFIED., .F., .F.,
 ( 4, 4 ),
 ( 2.380737581673561746E-07, 0.002336974151641583314 ),
 .UNSPECIFIED. ) ;
#16875 = CARTESIAN_POINT ( 'NONE',  ( -8.326672684688674053E-14, -2.000000000000029310, 8.000000000000076383 ) ) ;
#16876 = ORIENTED_EDGE ( 'NONE', *, *, #18893, .F. ) ;
#16877 = CARTESIAN_POINT ( 'NONE',  ( 4.132952817037863547, -4.063368025374519910, 2.081668171172168513E-14 ) ) ;
#16878 = DIRECTION ( 'NONE',  ( -0.000000000000000000, -0.000000000000000000, 1.000000000000000000 ) ) ;
#16879 = DIRECTION ( 'NONE',  ( -1.000000000000000000, 0.000000000000000000, 0.000000000000000000 ) ) ;
#16880 = PLANE ( 'NONE',  #830 ) ;
#16881 = EDGE_CURVE ( 'NONE', #16729, #13819, #17718, .T. ) ;
#16882 = CARTESIAN_POINT ( 'NONE',  ( -7.523705677351674836, -11.16164950472499484, 8.715168381931317043 ) ) ;
#16883 = CARTESIAN_POINT ( 'NONE',  ( -8.725359747074561412, -13.50000000719894011, 6.816426071237537521 ) ) ;
#16884 = DIRECTION ( 'NONE',  ( -5.551115123125818447E-17, 1.577721810442025713E-30, -1.000000000000000000 ) ) ;
#16885 = AXIS2_PLACEMENT_3D ( 'NONE', #4039, #18398, #14410 ) ;
#16886 = DIRECTION ( 'NONE',  ( -1.000000000000000000, 1.276756478318923119E-15, -1.333893503340766797E-15 ) ) ;
#16887 = LINE ( 'NONE', #2664, #15261 ) ;
#16888 =( LENGTH_UNIT ( ) NAMED_UNIT ( * ) SI_UNIT ( .MILLI., .METRE. ) );
#16889 = DIRECTION ( 'NONE',  ( -1.000000000000000000, -2.699383410053119644E-30, -3.330669073875432643E-16 ) ) ;
#16890 = FACE_OUTER_BOUND ( 'NONE', #22850, .T. ) ;
#16891 = ORIENTED_EDGE ( 'NONE', *, *, #2498, .F. ) ;
#16892 = ORIENTED_EDGE ( 'NONE', *, *, #13695, .T. ) ;
#16893 = VERTEX_POINT ( 'NONE', #5450 ) ;
#16894 = ORIENTED_EDGE ( 'NONE', *, *, #11706, .F. ) ;
#16895 = ORIENTED_EDGE ( 'NONE', *, *, #19140, .T. ) ;
#16896 = CARTESIAN_POINT ( 'NONE',  ( 25.60000000000000142, 0.000000000000000000, -6.938893903907228378E-15 ) ) ;
#16897 = CYLINDRICAL_SURFACE ( 'NONE', #17038, 0.5000000000000022204 ) ;
#16898 = VERTEX_POINT ( 'NONE', #23219 ) ;
#16899 = AXIS2_PLACEMENT_3D ( 'NONE', #4502, #20869, #18628 ) ;
#16900 = DIRECTION ( 'NONE',  ( -1.000000000000000000, 0.000000000000000000, 0.000000000000000000 ) ) ;
#16901 = CARTESIAN_POINT ( 'NONE',  ( 12.84999999999997300, -13.50000000000007105, 5.551115123125782702E-14 ) ) ;
#16902 = DIRECTION ( 'NONE',  ( -2.013525853228508439E-32, -6.779273404243028164E-31, 1.000000000000000000 ) ) ;
#16903 = EDGE_CURVE ( 'NONE', #5703, #8151, #1993, .T. ) ;
#16904 = CARTESIAN_POINT ( 'NONE',  ( -6.979889398549481427, 35.99999999900384751, -18.51271870087857607 ) ) ;
#16905 = FACE_OUTER_BOUND ( 'NONE', #14223, .T. ) ;
#16906 = CARTESIAN_POINT ( 'NONE',  ( 4.663380343546485562, 0.7500000000000558442, -2.264472787102512985 ) ) ;
#16907 = EDGE_CURVE ( 'NONE', #12006, #17574, #16261, .T. ) ;
#16908 = DIRECTION ( 'NONE',  ( 4.190823558986625216E-31, -1.000000000000000000, 4.190823558986625216E-31 ) ) ;
#16909 = CARTESIAN_POINT ( 'NONE',  ( -42.54314575050785407, -4.800000000000037126, -7.500000000000007105 ) ) ;
#16910 = PLANE ( 'NONE',  #8930 ) ;
#16911 = CARTESIAN_POINT ( 'NONE',  ( 2.775557561562891351E-14, 1.387778780781445676E-14, -9.999999999999968026 ) ) ;
#16912 = LINE ( 'NONE', #12816, #9325 ) ;
#16913 = CARTESIAN_POINT ( 'NONE',  ( 12.49999999999995914, 1.250000000000015099, -4.750000000000000888 ) ) ;
#16914 = EDGE_CURVE ( 'NONE', #20423, #13234, #15871, .T. ) ;
#16915 = CARTESIAN_POINT ( 'NONE',  ( 3.972066048304715213, -3.435565134476332716, -1.180968096049761495 ) ) ;
#16916 = CIRCLE ( 'NONE', #17681, 0.5000000000000000000 ) ;
#16917 = EDGE_LOOP ( 'NONE', ( #8053, #16979, #11780, #2268 ) ) ;
#16918 = VERTEX_POINT ( 'NONE', #5559 ) ;
#16919 = ADVANCED_FACE ( 'NONE', ( #3671, #1894 ), #5212, .T. ) ;
#16921 = ORIENTED_EDGE ( 'NONE', *, *, #14996, .T. ) ;
#16920 = EDGE_LOOP ( 'NONE', ( #13154, #21057, #5948, #15098 ) ) ;
#16922 = CARTESIAN_POINT ( 'NONE',  ( -6.999999999708142795, 38.99999999900385461, -22.50000000000000000 ) ) ;
#16923 = CARTESIAN_POINT ( 'NONE',  ( 3.333333333333280191, -2.694301256218290419, -3.300726591567090473 ) ) ;
#16924 = DIRECTION ( 'NONE',  ( -1.066786462891689527E-26, -6.656013887802287108E-31, -1.000000000000000000 ) ) ;
#16925 = ORIENTED_EDGE ( 'NONE', *, *, #1399, .T. ) ;
#16926 = TOROIDAL_SURFACE ( 'NONE', #19212, 4.500000000000000888, 0.5000000000000000000 ) ;
#16927 = DIRECTION ( 'NONE',  ( 0.7071067811865490160, 0.7071067811865460184, 1.565905175853766674E-16 ) ) ;
#16928 = DIRECTION ( 'NONE',  ( 0.000000000000000000, 0.000000000000000000, -1.000000000000000000 ) ) ;
#16929 = CARTESIAN_POINT ( 'NONE',  ( -4.499999999708154341, 35.99999999900384751, -19.50000000000000355 ) ) ;
#16930 = CARTESIAN_POINT ( 'NONE',  ( 119.5756419024615838, -11.00000000000006573, -6.000000000000116351 ) ) ;
#16931 = DIRECTION ( 'NONE',  ( 1.000000000000000000, 3.144186300207927518E-14, 0.000000000000000000 ) ) ;
#16932 = CARTESIAN_POINT ( 'NONE',  ( 119.5756419024615269, -11.00000000000006573, 6.000000000000081712 ) ) ;
#16933 = CARTESIAN_POINT ( 'NONE',  ( 6.500000000000283329, 2.500000000000168754, -5.999999999999943157 ) ) ;
#16934 = CARTESIAN_POINT ( 'NONE',  ( 8.529852775121097885E-15, 3.375361811986506755, -1.153701847711674278 ) ) ;
#16935 = SURFACE_STYLE_FILL_AREA ( #9666 ) ;
#16936 = CARTESIAN_POINT ( 'NONE',  ( 1.789509255758340803E-14, -3.375361811986531180, 1.153701847711657846 ) ) ;
#16937 = LINE ( 'NONE', #20732, #19416 ) ;
#16938 = ORIENTED_EDGE ( 'NONE', *, *, #16522, .F. ) ;
#16939 = SURFACE_STYLE_FILL_AREA ( #4599 ) ;
#16940 = CIRCLE ( 'NONE', #18470, 0.5000000000000038858 ) ;
#16941 = CIRCLE ( 'NONE', #19974, 10.34816708862279633 ) ;
#16943 = ORIENTED_EDGE ( 'NONE', *, *, #9860, .F. ) ;
#16942 = ORIENTED_EDGE ( 'NONE', *, *, #19160, .F. ) ;
#16944 = EDGE_CURVE ( 'NONE', #19930, #11087, #498, .T. ) ;
#16945 = EDGE_LOOP ( 'NONE', ( #23152, #11550, #13592, #7295 ) ) ;
#16947 = ORIENTED_EDGE ( 'NONE', *, *, #16103, .T. ) ;
#16946 = ORIENTED_EDGE ( 'NONE', *, *, #11153, .F. ) ;
#16948 = ORIENTED_EDGE ( 'NONE', *, *, #3936, .F. ) ;
#16949 = DIRECTION ( 'NONE',  ( 0.000000000000000000, 0.000000000000000000, -1.000000000000000000 ) ) ;
#16950 = CARTESIAN_POINT ( 'NONE',  ( 6.999999999999992006, 2.428612866367529932E-14, 11.74999999999996803 ) ) ;
#16951 = EDGE_LOOP ( 'NONE', ( #17216, #982 ) ) ;
#16952 = FACE_OUTER_BOUND ( 'NONE', #7098, .T. ) ;
#16953 = EDGE_CURVE ( 'NONE', #13979, #17272, #10944, .T. ) ;
#16954 = CARTESIAN_POINT ( 'NONE',  ( 0.3126073911696447549, -4.041451884327432076, 3.469446951953614189E-15 ) ) ;
#16955 = CARTESIAN_POINT ( 'NONE',  ( 2.775557561562891351E-14, 0.5000000000000004441, -6.499999999999950262 ) ) ;
#16956 = B_SPLINE_CURVE_WITH_KNOTS ( 'NONE', 3,
 ( #10675, #1843, #21846, #14545, #21737, #6777, #5623, #17976, #12782, #11131, #14663, #5736, #9031, #20086, #19615, #5395 ),
 .UNSPECIFIED., .F., .F.,
 ( 4, 2, 2, 2, 2, 2, 2, 4 ),
 ( 0.000000000000000000, 0.0004262889904590547608, 0.0008525779809181095216, 0.001278866971377164282, 0.001705155961836219043, 0.002131444952295272720, 0.002557733942754325963, 0.003410311923672432882 ),
 .UNSPECIFIED. ) ;
#16957 = CARTESIAN_POINT ( 'NONE',  ( 86.00000000000117950, -11.02760560296348125, 6.000000000000054179 ) ) ;
#16958 = EDGE_CURVE ( 'NONE', #3270, #16867, #18145, .T. ) ;
#16959 = DIRECTION ( 'NONE',  ( -6.621482934330023914E-16, -0.8660254037844379305, 0.5000000000000013323 ) ) ;
#16960 = DIRECTION ( 'NONE',  ( -1.000000000000000000, -6.640738306473676004E-15, -4.078150875473213127E-31 ) ) ;
#16961 = CARTESIAN_POINT ( 'NONE',  ( 7.467942433933822066, -2.153931645084771862, 7.356484134531140029 ) ) ;
#16962 = AXIS2_PLACEMENT_3D ( 'NONE', #15409, #22597, #8015 ) ;
#16963 = CIRCLE ( 'NONE', #15841, 7.499999999999998224 ) ;
#16964 = DIRECTION ( 'NONE',  ( 3.885780586188016830E-16, 4.437342591868156373E-31, -1.000000000000000000 ) ) ;
#16965 = LINE ( 'NONE', #17086, #7793 ) ;
#16966 = CARTESIAN_POINT ( 'NONE',  ( 2.499999999999988454, 4.500000000000059508, -1.250000000000028866 ) ) ;
#16967 = CARTESIAN_POINT ( 'NONE',  ( -0.4634555468559497515, 1.749999999999992673, -4.750000000000023093 ) ) ;
#16968 = DIRECTION ( 'NONE',  ( 0.000000000000000000, 0.000000000000000000, -1.000000000000000000 ) ) ;
#16969 = PRODUCT_DEFINITION_SHAPE ( 'NONE', 'NONE',  #23281 ) ;
#16970 = EDGE_LOOP ( 'NONE', ( #17707, #22068, #19703, #10458 ) ) ;
#16971 = EDGE_CURVE ( 'NONE', #14796, #17995, #9143, .T. ) ;
#16973 = ORIENTED_EDGE ( 'NONE', *, *, #5353, .T. ) ;
#16972 = EDGE_LOOP ( 'NONE', ( #21316, #6212, #826, #2553 ) ) ;
#16974 = EDGE_CURVE ( 'NONE', #235, #15346, #6138, .T. ) ;
#16975 = ORIENTED_EDGE ( 'NONE', *, *, #22353, .T. ) ;
#16976 = ORIENTED_EDGE ( 'NONE', *, *, #7575, .F. ) ;
#16977 = ORIENTED_EDGE ( 'NONE', *, *, #18805, .F. ) ;
#16978 = AXIS2_PLACEMENT_3D ( 'NONE', #10442, #3616, #6924 ) ;
#16979 = ORIENTED_EDGE ( 'NONE', *, *, #15480, .T. ) ;
#16980 = CARTESIAN_POINT ( 'NONE',  ( -66.55000000000046612, -7.593235069856354823E-14, -2.000000000000001776 ) ) ;
#16981 = EDGE_CURVE ( 'NONE', #10367, #11755, #19273, .T. ) ;
#16982 = ADVANCED_FACE ( 'NONE', ( #22013 ), #13190, .F. ) ;
#16983 = CARTESIAN_POINT ( 'NONE',  ( -57.28378781036000333, 2.700000000000098321, 8.541666666666698049 ) ) ;
#16984 = ORIENTED_EDGE ( 'NONE', *, *, #22881, .T. ) ;
#16985 = DIRECTION ( 'NONE',  ( 1.000000000000000000, -1.847414967615758933E-47, 3.885780586188017323E-16 ) ) ;
#16986 =( GEOMETRIC_REPRESENTATION_CONTEXT ( 3 ) GLOBAL_UNCERTAINTY_ASSIGNED_CONTEXT ( ( #22029 ) ) GLOBAL_UNIT_ASSIGNED_CONTEXT ( ( #18484, #18260, #15058 ) ) REPRESENTATION_CONTEXT ( 'NONE', 'WORKASPACE' ) );
#16987 = CARTESIAN_POINT ( 'NONE',  ( 0.000000000000000000, 0.5999999999999859890, -3.054668707061614086 ) ) ;
#16988 = FACE_OUTER_BOUND ( 'NONE', #14626, .T. ) ;
#16989 = FACE_OUTER_BOUND ( 'NONE', #9850, .T. ) ;
#16990 = CARTESIAN_POINT ( 'NONE',  ( -8.954763739086832430, -12.50000000000004263, 6.678571428571468793 ) ) ;
#16991 = DIRECTION ( 'NONE',  ( 0.000000000000000000, 0.000000000000000000, -1.000000000000000000 ) ) ;
#16992 = DIRECTION ( 'NONE',  ( -7.395570986446975166E-31, -3.382522293539642681E-32, -1.000000000000000000 ) ) ;
#16993 = TOROIDAL_SURFACE ( 'NONE', #10628, 5.750000000000000000, 0.5000000000000000000 ) ;
#16994 = LINE ( 'NONE', #15473, #8792 ) ;
#16995 = CIRCLE ( 'NONE', #16243, 2.549999999999997158 ) ;
#16996 = CARTESIAN_POINT ( 'NONE',  ( -42.54314575050785407, -7.500000000000038192, -7.500000000000007105 ) ) ;
#16997 = CIRCLE ( 'NONE', #20778, 7.000000000000000000 ) ;
#16998 = EDGE_CURVE ( 'NONE', #5016, #12512, #15509, .T. ) ;
#16999 = ORIENTED_EDGE ( 'NONE', *, *, #11667, .F. ) ;
#17000 = AXIS2_PLACEMENT_3D ( 'NONE', #148, #17789, #10490 ) ;
#17001 = EDGE_CURVE ( 'NONE', #19280, #11464, #2366, .T. ) ;
#17002 = EDGE_CURVE ( 'NONE', #20537, #1136, #18163, .T. ) ;
#17003 = CARTESIAN_POINT ( 'NONE',  ( -3.999999999708139686, 49.99999999900385461, -26.00000000000000711 ) ) ;
#17004 = ORIENTED_EDGE ( 'NONE', *, *, #16463, .T. ) ;
#17005 = ORIENTED_EDGE ( 'NONE', *, *, #18013, .F. ) ;
#17006 = ORIENTED_EDGE ( 'NONE', *, *, #3996, .T. ) ;
#17008 = ORIENTED_EDGE ( 'NONE', *, *, #9500, .F. ) ;
#17007 = EDGE_CURVE ( 'NONE', #9368, #16222, #21157, .T. ) ;
#17009 = ORIENTED_EDGE ( 'NONE', *, *, #1237, .F. ) ;
#17010 = CARTESIAN_POINT ( 'NONE',  ( 4.071447262713884463, 4.041451884327383226, 0.000000000000000000 ) ) ;
#17011 = CARTESIAN_POINT ( 'NONE',  ( 0.000000000000000000, 2.775557561562891351E-14, 17.49999999999997513 ) ) ;
#17012 = CIRCLE ( 'NONE', #514, 7.000000000000000000 ) ;
#17013 = ORIENTED_EDGE ( 'NONE', *, *, #9386, .F. ) ;
#17014 = EDGE_CURVE ( 'NONE', #10053, #17187, #3152, .T. ) ;
#17015 = VECTOR ( 'NONE', #19471, 1000.000000000000000 ) ;
#17016 = CARTESIAN_POINT ( 'NONE',  ( -7.500000000000020428, -8.000000000000017764, 10.24999999999999467 ) ) ;
#17017 = AXIS2_PLACEMENT_3D ( 'NONE', #15078, #640, #4930 ) ;
#17018 = AXIS2_PLACEMENT_3D ( 'NONE', #1298, #1404, #3635 ) ;
#17019 = CARTESIAN_POINT ( 'NONE',  ( 0.000000000000000000, 0.000000000000000000, 0.000000000000000000 ) ) ;
#17020 = CARTESIAN_POINT ( 'NONE',  ( 0.000000000000000000, 0.000000000000000000, 0.000000000000000000 ) ) ;
#17021 = VECTOR ( 'NONE', #3058, 1000.000000000000000 ) ;
#17022 = PRESENTATION_LAYER_ASSIGNMENT (  '', '', ( #3878 ) ) ;
#17023 = DIRECTION ( 'NONE',  ( -1.000000000000000000, -1.700709290173333260E-16, 0.000000000000000000 ) ) ;
#17024 = DIRECTION ( 'NONE',  ( -0.6819983600624940356, 0.7313537016191746787, 1.110361430785838977E-16 ) ) ;
#17025 = DIRECTION ( 'NONE',  ( 1.454462294001240516E-30, 1.000000000000000000, 0.000000000000000000 ) ) ;
#17026 = CARTESIAN_POINT ( 'NONE',  ( -12.85000000000001386, -12.00000000000006928, 4.163336342344337027E-14 ) ) ;
#17027 = DIRECTION ( 'NONE',  ( 9.693522803355793065E-26, -5.963788443470848352E-28, -1.000000000000000000 ) ) ;
#17028 = CARTESIAN_POINT ( 'NONE',  ( 83.98338480886823731, -11.64708151429766403, 6.500000000000117240 ) ) ;
#17029 = DIRECTION ( 'NONE',  ( 2.172745813409349776E-17, -1.000000000000000000, 1.309377075419428048E-16 ) ) ;
#17030 = DIRECTION ( 'NONE',  ( 2.775557561562891043E-17, -3.108639542312977099E-16, 1.000000000000000000 ) ) ;
#17031 = CARTESIAN_POINT ( 'NONE',  ( -89.70000000000059970, 0.5000000000000490719, 1.000000000000000888 ) ) ;
#17032 = CIRCLE ( 'NONE', #1292, 6.000000000000047073 ) ;
#17033 = SHAPE_REPRESENTATION ( 'Nut', ( #22115 ), #18753 ) ;
#17034 = LINE ( 'NONE', #20834, #4813 ) ;
#17035 = VECTOR ( 'NONE', #17553, 1000.000000000000000 ) ;
#17037 = ORIENTED_EDGE ( 'NONE', *, *, #10028, .F. ) ;
#17036 = AXIS2_PLACEMENT_3D ( 'NONE', #15257, #11965, #22451 ) ;
#17038 = AXIS2_PLACEMENT_3D ( 'NONE', #7973, #13269, #15140 ) ;
#17039 = CONTEXT_DEPENDENT_SHAPE_REPRESENTATION ( #545, #16969 ) ;
#17040 = ORIENTED_EDGE ( 'NONE', *, *, #5182, .F. ) ;
#17042 = ORIENTED_EDGE ( 'NONE', *, *, #7627, .F. ) ;
#17041 = EDGE_LOOP ( 'NONE', ( #12302, #20254, #8779, #16839 ) ) ;
#17043 = LINE ( 'NONE', #9888, #17021 ) ;
#17044 = EDGE_CURVE ( 'NONE', #14991, #3633, #11749, .T. ) ;
#17045 = DIRECTION ( 'NONE',  ( 1.000000000000000000, -4.190823558986610327E-31, 1.733449886265890494E-32 ) ) ;
#17046 = CARTESIAN_POINT ( 'NONE',  ( -0.5000000000000975886, -2.775557561562891351E-14, -7.500000000000007105 ) ) ;
#17047 = ORIENTED_EDGE ( 'NONE', *, *, #21203, .T. ) ;
#17048 = VECTOR ( 'NONE', #13430, 1000.000000000000000 ) ;
#17049 = CARTESIAN_POINT ( 'NONE',  ( -45.37157287525408833, -6.828427124746218269, -8.000000000000062172 ) ) ;
#17050 = FACE_OUTER_BOUND ( 'NONE', #15200, .T. ) ;
#17051 = AXIS2_PLACEMENT_3D ( 'NONE', #17099, #11820, #11927 ) ;
#17052 = CARTESIAN_POINT ( 'NONE',  ( -1.839530896184789155, 1.562503694739638016, 4.749999999999999112 ) ) ;
#17053 = DIRECTION ( 'NONE',  ( 1.000000000000000000, -7.100545512326564696E-57, -1.066786462891689527E-26 ) ) ;
#17054 = DIRECTION ( 'NONE',  ( 2.013525853228507892E-32, 6.902532920683810383E-31, -1.000000000000000000 ) ) ;
#17055 = CARTESIAN_POINT ( 'NONE',  ( 36.00000000029184832, 5.999999999003851059, -12.99999999999999822 ) ) ;
#17056 = LINE ( 'NONE', #22598, #7323 ) ;
#17057 = DIRECTION ( 'NONE',  ( 0.000000000000000000, 0.000000000000000000, 1.000000000000000000 ) ) ;
#17058 = CARTESIAN_POINT ( 'NONE',  ( -2.081668171172168513E-14, 2.000000000000001776, -1.250000000000001110 ) ) ;
#17059 = CARTESIAN_POINT ( 'NONE',  ( 10.50000000000000888, -13.50000000000003020, 6.250000000000033751 ) ) ;
#17060 = DIRECTION ( 'NONE',  ( -1.000000000000000000, 4.190823558986610327E-31, -1.733449886265890494E-32 ) ) ;
#17061 = LINE ( 'NONE', #10022, #22808 ) ;
#17062 = EDGE_LOOP ( 'NONE', ( #9062, #15719, #15369, #12264 ) ) ;
#17063 = AXIS2_PLACEMENT_3D ( 'NONE', #17286, #22596, #13542 ) ;
#17064 = CIRCLE ( 'NONE', #21615, 0.5000000000000004441 ) ;
#17066 = ORIENTED_EDGE ( 'NONE', *, *, #8442, .T. ) ;
#17065 = ORIENTED_EDGE ( 'NONE', *, *, #19285, .T. ) ;
#17067 = VERTEX_POINT ( 'NONE', #3894 ) ;
#17069 = ORIENTED_EDGE ( 'NONE', *, *, #4082, .T. ) ;
#17068 = ORIENTED_EDGE ( 'NONE', *, *, #6203, .T. ) ;
#17070 = EDGE_LOOP ( 'NONE', ( #5293, #21667, #13327, #5582, #15769 ) ) ;
#17071 = CARTESIAN_POINT ( 'NONE',  ( 0.2500000000000071609, 2.000000000000001776, -1.250000000000001110 ) ) ;
#17072 = ORIENTED_EDGE ( 'NONE', *, *, #10214, .F. ) ;
#17073 = ORIENTED_EDGE ( 'NONE', *, *, #9477, .T. ) ;
#17074 = FILL_AREA_STYLE ('',( #11668 ) ) ;
#17075 = FACE_OUTER_BOUND ( 'NONE', #10935, .T. ) ;
#17076 = DIRECTION ( 'NONE',  ( 0.7071067811865485719, -0.7071067811865464625, -1.010793663541191485E-16 ) ) ;
#17077 = CARTESIAN_POINT ( 'NONE',  ( -7.901093513163678139, -1.673173099260699903, 7.745538272134616875 ) ) ;
#17078 = AXIS2_PLACEMENT_3D ( 'NONE', #19505, #10788, #19381 ) ;
#17079 = CARTESIAN_POINT ( 'NONE',  ( 1.199999999999992628, 0.000000000000000000, 0.000000000000000000 ) ) ;
#17080 = CARTESIAN_POINT ( 'NONE',  ( 24.75000000000001066, 2.000000000000099032, -17.74999999999998224 ) ) ;
#17081 = CIRCLE ( 'NONE', #6974, 3.000000000000011546 ) ;
#17082 = CARTESIAN_POINT ( 'NONE',  ( 5.550000000291854363, 42.99999999900385461, -29.00000000000000355 ) ) ;
#17083 = DIRECTION ( 'NONE',  ( 1.000000000000000000, -1.424116703980815236E-16, -2.931272055834072201E-32 ) ) ;
#17084 = LINE ( 'NONE', #10157, #11334 ) ;
#17085 = EDGE_CURVE ( 'NONE', #16256, #1201, #2013, .T. ) ;
#17086 = CARTESIAN_POINT ( 'NONE',  ( -1.387778780781446464E-15, -3.004450713244089682E-31, 2.500000000000001332 ) ) ;
#17087 = DIRECTION ( 'NONE',  ( 0.000000000000000000, 3.469446951953622866E-15, 1.000000000000000000 ) ) ;
#17088 = CARTESIAN_POINT ( 'NONE',  ( -6.683546854663851455, 13.99327871316343952, -27.35588422962999999 ) ) ;
#17089 = CARTESIAN_POINT ( 'NONE',  ( 3.880198502136890770, 0.7307680362928052897, -3.500000000000006661 ) ) ;
#17090 = EDGE_LOOP ( 'NONE', ( #13589, #7763, #10864, #18999, #17357, #12445 ) ) ;
#17091 =( LENGTH_UNIT ( ) NAMED_UNIT ( * ) SI_UNIT ( .MILLI., .METRE. ) );
#17093 = ORIENTED_EDGE ( 'NONE', *, *, #13838, .F. ) ;
#17092 = ORIENTED_EDGE ( 'NONE', *, *, #81, .F. ) ;
#17094 = ORIENTED_EDGE ( 'NONE', *, *, #23064, .F. ) ;
#17095 = VERTEX_POINT ( 'NONE', #16699 ) ;
#17096 = VECTOR ( 'NONE', #15975, 1000.000000000000000 ) ;
#17097 = ORIENTED_EDGE ( 'NONE', *, *, #9824, .T. ) ;
#17098 = ORIENTED_EDGE ( 'NONE', *, *, #227, .F. ) ;
#17099 = CARTESIAN_POINT ( 'NONE',  ( 0.000000000000000000, 0.000000000000000000, 0.000000000000000000 ) ) ;
#17100 = AXIS2_PLACEMENT_3D ( 'NONE', #23216, #7104, #12834 ) ;
#17101 = DIRECTION ( 'NONE',  ( 1.454462294001240516E-30, 1.000000000000000000, 0.000000000000000000 ) ) ;
#17102 = ORIENTED_EDGE ( 'NONE', *, *, #3459, .T. ) ;
#17103 = EDGE_LOOP ( 'NONE', ( #13790, #5871, #23153, #5433, #5492, #2496 ) ) ;
#17104 = CARTESIAN_POINT ( 'NONE',  ( 119.5756419024615838, -11.00000000000006573, -6.000000000000116351 ) ) ;
#17105 = DIRECTION ( 'NONE',  ( -2.775557561562883647E-17, 3.652049423109057473E-16, -1.000000000000000000 ) ) ;
#17106 = ADVANCED_FACE ( 'NONE', ( #258 ), #9313, .T. ) ;
#17107 = CARTESIAN_POINT ( 'NONE',  ( -6.000000000000102141, 4.799999999999964295, 8.000000000000047962 ) ) ;
#17108 = CIRCLE ( 'NONE', #15608, 2.550000000000010481 ) ;
#17109 = FACE_OUTER_BOUND ( 'NONE', #17215, .T. ) ;
#17110 = CARTESIAN_POINT ( 'NONE',  ( -55.05572809000125289, 0.5000000000000143219, -10.00000000000006395 ) ) ;
#17111 = CARTESIAN_POINT ( 'NONE',  ( 4.142654963991856398, 4.070796997468703715, -6.519033156300609374E-18 ) ) ;
#17112 = EDGE_CURVE ( 'NONE', #9040, #15314, #14712, .T. ) ;
#17113 = CARTESIAN_POINT ( 'NONE',  ( -4.000000000000045297, 1.387778780781445676E-14, 0.000000000000000000 ) ) ;
#17114 = DIRECTION ( 'NONE',  ( -1.095614826932724588E-15, -6.741645191078037727E-32, 1.000000000000000000 ) ) ;
#17115 = DIRECTION ( 'NONE',  ( -0.000000000000000000, -0.000000000000000000, -1.000000000000000000 ) ) ;
#17116 = CARTESIAN_POINT ( 'NONE',  ( 37.86602540378474657, -6.071532165918824830E-15, -10.86602540378446058 ) ) ;
#17117 = ORIENTED_EDGE ( 'NONE', *, *, #18450, .T. ) ;
#17118 = ADVANCED_FACE ( 'NONE', ( #22128 ), #6019, .F. ) ;
#17119 = CARTESIAN_POINT ( 'NONE',  ( 3.958484000407115122, 3.734437307742082268, 0.5317648453099944605 ) ) ;
#17120 = CARTESIAN_POINT ( 'NONE',  ( 10.49999999999998224, -12.00000000000000711, 9.250000000000021316 ) ) ;
#17121 = EDGE_CURVE ( 'NONE', #22677, #5239, #16874, .T. ) ;
#17122 = ORIENTED_EDGE ( 'NONE', *, *, #18026, .F. ) ;
#17123 = ADVANCED_FACE ( 'NONE', ( #18373 ), #4824, .T. ) ;
#17124 = CIRCLE ( 'NONE', #7015, 0.5000000000000022204 ) ;
#17125 = ORIENTED_EDGE ( 'NONE', *, *, #4491, .T. ) ;
#17126 = EDGE_LOOP ( 'NONE', ( #1353, #8343, #5201 ) ) ;
#17127 = ORIENTED_EDGE ( 'NONE', *, *, #5574, .F. ) ;
#17128 = ORIENTED_EDGE ( 'NONE', *, *, #12716, .F. ) ;
#17129 = LINE ( 'NONE', #20453, #18128 ) ;
#17130 = DIRECTION ( 'NONE',  ( -1.550910762415566494E-16, -1.000000000000000000, 8.135128085091684243E-31 ) ) ;
#17131 = ORIENTED_EDGE ( 'NONE', *, *, #1210, .T. ) ;
#17132 = CARTESIAN_POINT ( 'NONE',  ( 0.000000000000000000, 0.000000000000000000, -5.000000000000000888 ) ) ;
#17133 = CYLINDRICAL_SURFACE ( 'NONE', #12265, 0.5000000000000028866 ) ;
#17134 = CARTESIAN_POINT ( 'NONE',  ( -42.54314575050782565, -4.000000000000034639, -8.000000000000007105 ) ) ;
#17135 = EDGE_CURVE ( 'NONE', #8641, #9717, #15291, .T. ) ;
#17136 = CIRCLE ( 'NONE', #7025, 0.5000000000000029976 ) ;
#17137 = CARTESIAN_POINT ( 'NONE',  ( -50.65685424949267457, -7.200000000000049916, 7.500000000000047962 ) ) ;
#17138 = DIRECTION ( 'NONE',  ( 0.000000000000000000, 0.000000000000000000, 1.000000000000000000 ) ) ;
#17139 = DIRECTION ( 'NONE',  ( -4.190823558986625216E-31, 1.000000000000000000, -4.190823558986625216E-31 ) ) ;
#17140 = AXIS2_PLACEMENT_3D ( 'NONE', #16996, #6321, #11835 ) ;
#17141 = CARTESIAN_POINT ( 'NONE',  ( 59.19834661797866460, 2.499999999999946709, 6.500000000000130562 ) ) ;
#17142 = CARTESIAN_POINT ( 'NONE',  ( 2.775557561562891351E-14, 3.000000000000006217, -6.499999999999950262 ) ) ;
#17143 = MECHANICAL_DESIGN_GEOMETRIC_PRESENTATION_REPRESENTATION (  '', ( #15264 ), #18505 ) ;
#17144 = DIRECTION ( 'NONE',  ( 1.454462294001240516E-30, 1.000000000000000000, 0.000000000000000000 ) ) ;
#17145 = CIRCLE ( 'NONE', #11520, 0.4999999999999995559 ) ;
#17146 = FACE_OUTER_BOUND ( 'NONE', #6009, .T. ) ;
#17147 = EDGE_CURVE ( 'NONE', #23201, #16369, #8364, .T. ) ;
#17148 = LINE ( 'NONE', #2931, #2104 ) ;
#17149 = EDGE_CURVE ( 'NONE', #20996, #15911, #22292, .T. ) ;
#17150 = CARTESIAN_POINT ( 'NONE',  ( 22.49999999999993960, 4.250000000000045297, -17.50000000000001066 ) ) ;
#17151 = ORIENTED_EDGE ( 'NONE', *, *, #3735, .F. ) ;
#17152 = EDGE_CURVE ( 'NONE', #5983, #20043, #13425, .T. ) ;
#17153 = VECTOR ( 'NONE', #12240, 1000.000000000000000 ) ;
#17154 = CONTEXT_DEPENDENT_SHAPE_REPRESENTATION ( #21864, #12103 ) ;
#17155 = ORIENTED_EDGE ( 'NONE', *, *, #16464, .T. ) ;
#17156 = AXIS2_PLACEMENT_3D ( 'NONE', #16861, #20766, #22522 ) ;
#17157 = AXIS2_PLACEMENT_3D ( 'NONE', #18835, #2711, #22599 ) ;
#17159 = ORIENTED_EDGE ( 'NONE', *, *, #12227, .T. ) ;
#17158 = ORIENTED_EDGE ( 'NONE', *, *, #15687, .T. ) ;
#17160 = DIRECTION ( 'NONE',  ( 5.551115123561405253E-17, 1.000000000000000000, -5.963788443470795439E-28 ) ) ;
#17161 = CARTESIAN_POINT ( 'NONE',  ( -50.65685424949274562, -0.5000000000001045830, 8.000000000000062172 ) ) ;
#17162 = PLANE ( 'NONE',  #3383 ) ;
#17163 = VECTOR ( 'NONE', #8687, 1000.000000000000000 ) ;
#17164 = ORIENTED_EDGE ( 'NONE', *, *, #10677, .F. ) ;
#17165 = DIRECTION ( 'NONE',  ( -1.000000000000000000, 0.000000000000000000, 0.000000000000000000 ) ) ;
#17166 = DIRECTION ( 'NONE',  ( 0.2405376366294412205, 0.000000000000000000, -0.9706398123736338368 ) ) ;
#17167 = CARTESIAN_POINT ( 'NONE',  ( 2.775557561562891351E-14, 10.99999999999998579, -2.133974596215532316 ) ) ;
#17168 = DIRECTION ( 'NONE',  ( 1.000000000000000000, 6.224605580259554159E-31, -2.887593071917436153E-31 ) ) ;
#17169 = CARTESIAN_POINT ( 'NONE',  ( 115.1426525620553036, -6.246200939475421876, 6.500000000000137668 ) ) ;
#17170 = DIRECTION ( 'NONE',  ( 0.000000000000000000, 0.000000000000000000, -1.000000000000000000 ) ) ;
#17171 = AXIS2_PLACEMENT_3D ( 'NONE', #18457, #7640, #13287 ) ;
#17172 = FACE_OUTER_BOUND ( 'NONE', #18171, .T. ) ;
#17173 = CARTESIAN_POINT ( 'NONE',  ( 35.50000000029184832, -9.961476088449217059E-10, -19.00000000000000355 ) ) ;
#17174 = EDGE_CURVE ( 'NONE', #4432, #15682, #12134, .T. ) ;
#17175 = DIRECTION ( 'NONE',  ( 0.000000000000000000, 0.000000000000000000, 1.000000000000000000 ) ) ;
#17176 = CIRCLE ( 'NONE', #20960, 2.054999999999999716 ) ;
#17177 = DIRECTION ( 'NONE',  ( 7.860214984770699307E-18, -1.409037165336591006E-16, -1.000000000000000000 ) ) ;
#17178 = LINE ( 'NONE', #22138, #20242 ) ;
#17179 = AXIS2_PLACEMENT_3D ( 'NONE', #3536, #5295, #5648 ) ;
#17180 = CARTESIAN_POINT ( 'NONE',  ( 33.59619407800440882, 21.59619407671641866, -18.50000000000000355 ) ) ;
#17181 = EDGE_CURVE ( 'NONE', #9160, #5703, #9893, .T. ) ;
#17182 = ORIENTED_EDGE ( 'NONE', *, *, #8529, .F. ) ;
#17183 = TOROIDAL_SURFACE ( 'NONE', #19441, 5.750000000000000000, 0.5000000000000000000 ) ;
#17184 = SHAPE_REPRESENTATION_RELATIONSHIP ( 'NONE' , 'NONE' ,  #17992, #2433 ) ;
#17186 = ORIENTED_EDGE ( 'NONE', *, *, #6550, .T. ) ;
#17185 = EDGE_LOOP ( 'NONE', ( #19395, #10169, #19031, #10121, #19763, #13714, #1525, #3057, #8061, #16031, #11346, #5611 ) ) ;
#17187 = VERTEX_POINT ( 'NONE', #22370 ) ;
#17189 = VERTEX_POINT ( 'NONE', #13887 ) ;
#17188 = VERTEX_POINT ( 'NONE', #13658 ) ;
#17190 = VECTOR ( 'NONE', #6347, 1000.000000000000000 ) ;
#17191 = VERTEX_POINT ( 'NONE', #17167 ) ;
#17192 = CARTESIAN_POINT ( 'NONE',  ( 3.972709601346574360, 3.429395227388265521, 1.191688283765287348 ) ) ;
#17193 = AXIS2_PLACEMENT_3D ( 'NONE', #1830, #10658, #21496 ) ;
#17194 = DIRECTION ( 'NONE',  ( 1.000000000000000000, 0.000000000000000000, 2.668805347656595124E-16 ) ) ;
#17195 = PRESENTATION_STYLE_ASSIGNMENT (( #22510 ) ) ;
#17196 = DIRECTION ( 'NONE',  ( -1.000000000000000000, -1.479114197289397135E-31, -5.916456789157588541E-31 ) ) ;
#17197 = CIRCLE ( 'NONE', #5952, 0.4999999999999994449 ) ;
#17198 = DIRECTION ( 'NONE',  ( -1.000000000000000000, 4.615739097524200579E-16, -1.134196829589822059E-15 ) ) ;
#17199 = DIRECTION ( 'NONE',  ( 5.551115123561405253E-17, 1.000000000000000000, 2.256980353643891447E-27 ) ) ;
#17200 = PRESENTATION_LAYER_ASSIGNMENT (  '', '', ( #7812 ) ) ;
#17201 = CARTESIAN_POINT ( 'NONE',  ( 4.071447262713884463, -2.020725942163688504, 3.499999999999997780 ) ) ;
#17202 = CARTESIAN_POINT ( 'NONE',  ( 3.999999999999980016, 1.680228229147109786, -3.316631783032607750 ) ) ;
#17203 = AXIS2_PLACEMENT_3D ( 'NONE', #21199, #14123, #16342 ) ;
#17204 = CARTESIAN_POINT ( 'NONE',  ( 7.670621117724478744, -2.511599330829040966, 8.215271161873941352 ) ) ;
#17205 = DIRECTION ( 'NONE',  ( 1.000000000000000000, 1.424116703980846297E-16, -1.095779650622964657E-32 ) ) ;
#17206 = ADVANCED_FACE ( 'NONE', ( #15640 ), #10260, .T. ) ;
#17207 = CARTESIAN_POINT ( 'NONE',  ( -64.00000000000045475, 6.245004513516505540E-14, -1.999999999999974021 ) ) ;
#17208 = CARTESIAN_POINT ( 'NONE',  ( -7.884991313526915846, -12.31730826388680455, 7.773664271103684520 ) ) ;
#17209 = CARTESIAN_POINT ( 'NONE',  ( 0.000000000000000000, -1.750000000000001554, 0.000000000000000000 ) ) ;
#17210 = DIRECTION ( 'NONE',  ( -1.000000000000000000, -2.220446049250314067E-16, 5.825996348268307008E-33 ) ) ;
#17211 = EDGE_CURVE ( 'NONE', #9718, #226, #14643, .T. ) ;
#17212 = CIRCLE ( 'NONE', #14962, 0.5000000000000029976 ) ;
#17213 = ORIENTED_EDGE ( 'NONE', *, *, #19283, .F. ) ;
#17214 =( NAMED_UNIT ( * ) PLANE_ANGLE_UNIT ( ) SI_UNIT ( $, .RADIAN. ) );
#17216 = ORIENTED_EDGE ( 'NONE', *, *, #1173, .T. ) ;
#17215 = EDGE_LOOP ( 'NONE', ( #2241, #20426, #22559, #3600 ) ) ;
#17217 = ORIENTED_EDGE ( 'NONE', *, *, #9991, .F. ) ;
#17218 = TOROIDAL_SURFACE ( 'NONE', #3710, 6.500000000000000888, 0.5000000000000000000 ) ;
#17219 = ORIENTED_EDGE ( 'NONE', *, *, #22981, .T. ) ;
#17220 = VECTOR ( 'NONE', #7472, 1000.000000000000000 ) ;
#17221 = ORIENTED_EDGE ( 'NONE', *, *, #14300, .F. ) ;
#17222 = EDGE_CURVE ( 'NONE', #22610, #13451, #3853, .T. ) ;
#17223 = VERTEX_POINT ( 'NONE', #16929 ) ;
#17224 = DIRECTION ( 'NONE',  ( 0.000000000000000000, 0.000000000000000000, 1.000000000000000000 ) ) ;
#17225 = LINE ( 'NONE', #4405, #9883 ) ;
#17226 = VERTEX_POINT ( 'NONE', #18955 ) ;
#17227 = CARTESIAN_POINT ( 'NONE',  ( 6.000000000291855429, 2.999999999003851503, -39.00000000000000000 ) ) ;
#17228 =( GEOMETRIC_REPRESENTATION_CONTEXT ( 3 ) GLOBAL_UNCERTAINTY_ASSIGNED_CONTEXT ( ( #1328 ) ) GLOBAL_UNIT_ASSIGNED_CONTEXT ( ( #920, #14307, #5257 ) ) REPRESENTATION_CONTEXT ( 'NONE', 'WORKASPACE' ) );
#17229 = DIRECTION ( 'NONE',  ( 1.066786462891689527E-26, 6.656013887802287108E-31, 1.000000000000000000 ) ) ;
#17230 = CARTESIAN_POINT ( 'NONE',  ( 2.775557561562891351E-14, 8.000000000000003553, -6.499999999999950262 ) ) ;
#17231 = CARTESIAN_POINT ( 'NONE',  ( -50.65685424949262483, -7.200000000000071232, -16.89924331519437928 ) ) ;
#17232 = DIRECTION ( 'NONE',  ( 0.9706398123736300620, 1.281898970984135951E-30, 0.2405376366294562085 ) ) ;
#17233 = DIRECTION ( 'NONE',  ( -1.000000000000000000, 0.000000000000000000, 1.613696256722611405E-16 ) ) ;
#17234 = DIRECTION ( 'NONE',  ( -1.000000000000000000, -2.699383410053119644E-30, -3.330669073875432643E-16 ) ) ;
#17235 = CARTESIAN_POINT ( 'NONE',  ( -12.85000000000001386, -14.00000000000007105, 5.551115123125782702E-14 ) ) ;
#17236 = CIRCLE ( 'NONE', #7129, 0.5000000000000028866 ) ;
#17237 = CARTESIAN_POINT ( 'NONE',  ( -89.70000000000048601, -2.700000000000084110, 1.000000000000000888 ) ) ;
#17238 = DIRECTION ( 'NONE',  ( 1.000000000000000000, 1.424116703980846297E-16, -1.095779650622964657E-32 ) ) ;
#17239 = VERTEX_POINT ( 'NONE', #15177 ) ;
#17240 = CARTESIAN_POINT ( 'NONE',  ( 0.000000000000000000, 0.000000000000000000, 0.000000000000000000 ) ) ;
#17241 = DIRECTION ( 'NONE',  ( 0.000000000000000000, -6.938893903907237844E-15, -1.000000000000000000 ) ) ;
#17242 = ORIENTED_EDGE ( 'NONE', *, *, #10839, .T. ) ;
#17243 = ORIENTED_EDGE ( 'NONE', *, *, #4167, .F. ) ;
#17244 = EDGE_LOOP ( 'NONE', ( #8060, #15191, #7339, #8530 ) ) ;
#17245 = ORIENTED_EDGE ( 'NONE', *, *, #2958, .T. ) ;
#17246 = ORIENTED_EDGE ( 'NONE', *, *, #12419, .T. ) ;
#17247 = EDGE_CURVE ( 'NONE', #9421, #18277, #19656, .T. ) ;
#17248 = CARTESIAN_POINT ( 'NONE',  ( 4.071447262713884463, 2.020725942163688504, 3.499999999999997780 ) ) ;
#17249 = ORIENTED_EDGE ( 'NONE', *, *, #5098, .T. ) ;
#17250 = PLANE ( 'NONE',  #4967 ) ;
#17251 = DIRECTION ( 'NONE',  ( -9.121204216617949000E-31, -1.000000000000000000, 6.982962677686261977E-15 ) ) ;
#17252 = CARTESIAN_POINT ( 'NONE',  ( 2.499999999999992006, 2.000000000000001776, -1.250000000000028866 ) ) ;
#17253 = PRODUCT_RELATED_PRODUCT_CATEGORY ( 'part', '', ( #20565 ) ) ;
#17254 = ADVANCED_FACE ( 'NONE', ( #11993 ), #12884, .T. ) ;
#17255 = FACE_OUTER_BOUND ( 'NONE', #11870, .T. ) ;
#17256 = CARTESIAN_POINT ( 'NONE',  ( 108.9540049198142100, -11.33354449810597409, 6.500000000000040856 ) ) ;
#17257 = AXIS2_PLACEMENT_3D ( 'NONE', #17227, #1137, #13715 ) ;
#17258 = B_SPLINE_CURVE_WITH_KNOTS ( 'NONE', 3,
 ( #18543, #2425, #22313, #20315 ),
 .UNSPECIFIED., .F., .F.,
 ( 4, 4 ),
 ( 0.004330357959029834669, 0.008660484977952034868 ),
 .UNSPECIFIED. ) ;
#17259 = DIRECTION ( 'NONE',  ( -1.000000000000000000, 4.190823558986610327E-31, -1.733449886265890494E-32 ) ) ;
#17260 = EDGE_CURVE ( 'NONE', #14890, #12565, #9506, .T. ) ;
#17261 = AXIS2_PLACEMENT_3D ( 'NONE', #1097, #20380, #8264 ) ;
#17262 = LINE ( 'NONE', #8225, #2063 ) ;
#17263 = LINE ( 'NONE', #4692, #17953 ) ;
#17264 = DIRECTION ( 'NONE',  ( -3.330669073875432643E-16, -4.437342591868153746E-31, 1.000000000000000000 ) ) ;
#17265 = PLANE ( 'NONE',  #5913 ) ;
#17266 = CARTESIAN_POINT ( 'NONE',  ( 12.49999999999995914, 2.775557561562891036E-14, -14.50000000000000355 ) ) ;
#17267 = CARTESIAN_POINT ( 'NONE',  ( -4.000000000000107470, 2.309401076758546445, -0.4999999999999865663 ) ) ;
#17268 = ORIENTED_EDGE ( 'NONE', *, *, #1681, .T. ) ;
#17269 = EDGE_CURVE ( 'NONE', #5235, #9785, #17285, .T. ) ;
#17270 = EDGE_CURVE ( 'NONE', #18651, #13735, #6599, .T. ) ;
#17271 = CIRCLE ( 'NONE', #386, 0.5000000000000034417 ) ;
#17272 = VERTEX_POINT ( 'NONE', #19179 ) ;
#17273 = EDGE_CURVE ( 'NONE', #343, #2319, #135, .T. ) ;
#17275 = VERTEX_POINT ( 'NONE', #7305 ) ;
#17274 = ORIENTED_EDGE ( 'NONE', *, *, #3171, .F. ) ;
#17276 = DIRECTION ( 'NONE',  ( -1.000000000000000000, -2.168404344971017743E-16, 1.780660105995169760E-30 ) ) ;
#17277 = EDGE_CURVE ( 'NONE', #14161, #17189, #6760, .T. ) ;
#17278 = CARTESIAN_POINT ( 'NONE',  ( 2.775557561562891351E-14, 2.999999999999999112, -6.499999999999950262 ) ) ;
#17279 = CARTESIAN_POINT ( 'NONE',  ( 5.599999999999994316, 2.020725942163688504, -3.500000000000005773 ) ) ;
#17281 = VERTEX_POINT ( 'NONE', #1653 ) ;
#17280 = EDGE_CURVE ( 'NONE', #15772, #22002, #18555, .T. ) ;
#17282 = CARTESIAN_POINT ( 'NONE',  ( -6.000000000000116351, 7.499999999999958256, -7.500000000000062172 ) ) ;
#17283 = CARTESIAN_POINT ( 'NONE',  ( -12.84999999999999964, -1.500000000000001332, 5.750000000000005329 ) ) ;
#17284 = EDGE_CURVE ( 'NONE', #17687, #19001, #19975, .T. ) ;
#17285 = LINE ( 'NONE', #22719, #4232 ) ;
#17286 = CARTESIAN_POINT ( 'NONE',  ( 0.000000000000000000, 0.000000000000000000, 0.000000000000000000 ) ) ;
#17287 = CIRCLE ( 'NONE', #5660, 0.2500000000000000000 ) ;
#17288 = FACE_OUTER_BOUND ( 'NONE', #23245, .T. ) ;
#17289 = DIRECTION ( 'NONE',  ( 1.000000000000000000, -6.640738306473671271E-15, -4.480856046118915636E-31 ) ) ;
#17290 = CARTESIAN_POINT ( 'NONE',  ( -3.674234614174765046, 0.7500000000000630607, -2.999999999999995559 ) ) ;
#17291 = B_SPLINE_CURVE_WITH_KNOTS ( 'NONE', 3,
 ( #14859, #8034, #11090, #9338, #9682, #22267, #13209, #12985 ),
 .UNSPECIFIED., .F., .F.,
 ( 4, 2, 2, 4 ),
 ( 0.002775112046897000757, 0.003466237704215407826, 0.004157363361533814028, 0.005539614676170626431 ),
 .UNSPECIFIED. ) ;
#17292 =( LENGTH_UNIT ( ) NAMED_UNIT ( * ) SI_UNIT ( .MILLI., .METRE. ) );
#17293 = EDGE_CURVE ( 'NONE', #20569, #18939, #5425, .T. ) ;
#17294 = ORIENTED_EDGE ( 'NONE', *, *, #23203, .F. ) ;
#17295 = ADVANCED_FACE ( 'NONE', ( #6831 ), #4935, .F. ) ;
#17296 = DIRECTION ( 'NONE',  ( 0.9257916064627956798, 0.3780342595625901247, -4.196974335475888572E-17 ) ) ;
#17298 = ORIENTED_EDGE ( 'NONE', *, *, #22881, .F. ) ;
#17297 = VERTEX_POINT ( 'NONE', #19406 ) ;
#17299 = UNCERTAINTY_MEASURE_WITH_UNIT (LENGTH_MEASURE( 1.000000000000000082E-05 ), #5172, 'distance_accuracy_value', 'NONE');
#17300 = ORIENTED_EDGE ( 'NONE', *, *, #9307, .F. ) ;
#17302 = ORIENTED_EDGE ( 'NONE', *, *, #9672, .T. ) ;
#17301 = VERTEX_POINT ( 'NONE', #12583 ) ;
#17303 = AXIS2_PLACEMENT_3D ( 'NONE', #1416, #4712, #21192 ) ;
#17304 = ORIENTED_EDGE ( 'NONE', *, *, #17939, .F. ) ;
#17305 = ADVANCED_FACE ( 'NONE', ( #10702 ), #10474, .T. ) ;
#17306 = CARTESIAN_POINT ( 'NONE',  ( 6.495190528383258943, -8.326672684688674053E-14, 3.749999999999961808 ) ) ;
#17307 = FACE_OUTER_BOUND ( 'NONE', #15454, .T. ) ;
#17308 = CARTESIAN_POINT ( 'NONE',  ( 5.551115123125782702E-14, 0.2500000000000002220, -2.566987298107781257 ) ) ;
#17309 = DIRECTION ( 'NONE',  ( 1.454462294001240516E-30, 1.000000000000000000, 0.000000000000000000 ) ) ;
#17310 = DIRECTION ( 'NONE',  ( 1.000000000000000000, 2.699383410053120695E-30, 3.885780586188017323E-16 ) ) ;
#17311 = CARTESIAN_POINT ( 'NONE',  ( 111.3116192909783138, -9.818697260249948044, -6.500000000000047073 ) ) ;
#17312 = DIRECTION ( 'NONE',  ( 0.000000000000000000, -1.000000000000000000, 0.000000000000000000 ) ) ;
#17313 = DIRECTION ( 'NONE',  ( 1.000000000000000000, 0.000000000000000000, 0.000000000000000000 ) ) ;
#17314 = EDGE_CURVE ( 'NONE', #20860, #3634, #14119, .T. ) ;
#17315 = DIRECTION ( 'NONE',  ( 0.000000000000000000, -1.224646799147353947E-16, 1.000000000000000000 ) ) ;
#17316 = CARTESIAN_POINT ( 'NONE',  ( -47.47487373415322764, -4.018019484660590557, 8.000000000000145661 ) ) ;
#17317 = DIRECTION ( 'NONE',  ( 0.000000000000000000, -6.162975822039153854E-31, -1.000000000000000000 ) ) ;
#17318 = CARTESIAN_POINT ( 'NONE',  ( 4.113620667976089607, 1.749999999999973799, 2.375000000000000444 ) ) ;
#17319 = LINE ( 'NONE', #17558, #13064 ) ;
#17320 = VECTOR ( 'NONE', #3834, 1000.000000000000000 ) ;
#17321 = VECTOR ( 'NONE', #12966, 1000.000000000000000 ) ;
#17322 = CARTESIAN_POINT ( 'NONE',  ( -5.281014309470088541, 13.78823385074812613, -28.71965152573269719 ) ) ;
#17323 = FACE_OUTER_BOUND ( 'NONE', #6976, .T. ) ;
#17324 = ORIENTED_EDGE ( 'NONE', *, *, #9390, .T. ) ;
#17325 =( NAMED_UNIT ( * ) SI_UNIT ( $, .STERADIAN. ) SOLID_ANGLE_UNIT ( ) );
#17327 = EDGE_LOOP ( 'NONE', ( #20183, #6150, #21445, #518 ) ) ;
#17326 = EDGE_LOOP ( 'NONE', ( #12895, #18592, #1469, #17682 ) ) ;
#17328 = ORIENTED_EDGE ( 'NONE', *, *, #6054, .F. ) ;
#17329 = ORIENTED_EDGE ( 'NONE', *, *, #1601, .F. ) ;
#17330 = ORIENTED_EDGE ( 'NONE', *, *, #7212, .T. ) ;
#17331 = EDGE_CURVE ( 'NONE', #14653, #5722, #8709, .T. ) ;
#17332 = AXIS2_PLACEMENT_3D ( 'NONE', #9700, #20526, #11330 ) ;
#17333 = ORIENTED_EDGE ( 'NONE', *, *, #19879, .F. ) ;
#17334 = CYLINDRICAL_SURFACE ( 'NONE', #4676, 0.5000000000000004441 ) ;
#17335 = CONICAL_SURFACE ( 'NONE', #1203, 5.371010071662833063, 1.221730476396037490 ) ;
#17336 = AXIS2_PLACEMENT_3D ( 'NONE', #22219, #578, #9984 ) ;
#17337 = DIRECTION ( 'NONE',  ( 2.013525853228507892E-32, 6.902532920683810383E-31, -1.000000000000000000 ) ) ;
#17338 = ORIENTED_EDGE ( 'NONE', *, *, #1199, .T. ) ;
#17339 = DIRECTION ( 'NONE',  ( -1.000000000000000000, 1.276756478318922725E-15, -1.333893503340766402E-15 ) ) ;
#17340 = EDGE_CURVE ( 'NONE', #16493, #5042, #5775, .T. ) ;
#17341 = DIRECTION ( 'NONE',  ( 1.134196829589822059E-15, 6.741645191078037727E-32, -1.000000000000000000 ) ) ;
#17342 = B_SPLINE_CURVE_WITH_KNOTS ( 'NONE', 3,
 ( #11364, #7852, #14793, #685, #22205, #335 ),
 .UNSPECIFIED., .F., .F.,
 ( 4, 2, 4 ),
 ( 0.005852013090620628716, 0.006875955131657974020, 0.007899897172695319325 ),
 .UNSPECIFIED. ) ;
#17343 = CARTESIAN_POINT ( 'NONE',  ( 29.00000000029184832, 16.99999999900385461, -19.49999999999998934 ) ) ;
#17344 = DIRECTION ( 'NONE',  ( -9.121204216617949000E-31, -1.000000000000000000, 6.982962677686261977E-15 ) ) ;
#17345 = CARTESIAN_POINT ( 'NONE',  ( 112.6756160111033722, -11.28140466348826010, -6.000000000000047073 ) ) ;
#17346 = DIRECTION ( 'NONE',  ( -0.7313537016191715701, 0.6819983600624975884, 1.072890437865588353E-16 ) ) ;
#17347 = CARTESIAN_POINT ( 'NONE',  ( 57.15235153779114796, -1.074585193523325266, 6.000000000000185629 ) ) ;
#17348 = PLANE ( 'NONE',  #2581 ) ;
#17349 = CIRCLE ( 'NONE', #9858, 1.750000000000000000 ) ;
#17350 = DIRECTION ( 'NONE',  ( 1.000000000000000000, -2.168404344971005170E-16, 1.203141491611682442E-30 ) ) ;
#17351 = DIRECTION ( 'NONE',  ( -1.000000000000000000, 1.734723475976809806E-16, 5.551115123125699502E-17 ) ) ;
#17352 = ORIENTED_EDGE ( 'NONE', *, *, #2070, .F. ) ;
#17353 = FILL_AREA_STYLE_COLOUR ( '', #15699 ) ;
#17354 = DIRECTION ( 'NONE',  ( 0.000000000000000000, -1.000000000000000000, 0.000000000000000000 ) ) ;
#17355 = CARTESIAN_POINT ( 'NONE',  ( 6.500000000000339284, 0.5000000000001392220, -6.499999999999957367 ) ) ;
#17356 = VECTOR ( 'NONE', #16640, 1000.000000000000000 ) ;
#17357 = ORIENTED_EDGE ( 'NONE', *, *, #13250, .T. ) ;
#17358 = ORIENTED_EDGE ( 'NONE', *, *, #22199, .T. ) ;
#17359 = ORIENTED_EDGE ( 'NONE', *, *, #21959, .T. ) ;
#17360 = PRODUCT ( 'hex nut gradec_bsi_BS EN 24034 - M5 - N', 'hex nut gradec_bsi_BS EN 24034 - M5 - N', '', ( #3762 ) ) ;
#17361 = ORIENTED_EDGE ( 'NONE', *, *, #4244, .T. ) ;
#17362 = CARTESIAN_POINT ( 'NONE',  ( -42.54314575050781144, -3.999999999999996447, -16.42537846091818210 ) ) ;
#17363 = CARTESIAN_POINT ( 'NONE',  ( -2.000000000000015543, -3.464101615137743728, 0.000000000000000000 ) ) ;
#17364 = ORIENTED_EDGE ( 'NONE', *, *, #22216, .F. ) ;
#17365 = STYLED_ITEM ( 'NONE', ( #13431 ), #5581 ) ;
#17366 = DIRECTION ( 'NONE',  ( 5.551115123125790098E-17, 6.982962677686276177E-15, 1.000000000000000000 ) ) ;
#17367 = CARTESIAN_POINT ( 'NONE',  ( 42.50000000000014921, 0.000000000000000000, -12.49999999999998401 ) ) ;
#17368 = CARTESIAN_POINT ( 'NONE',  ( -52.60445557845689990, 9.020562075079396891E-14, 15.85914177512520773 ) ) ;
#17369 = LINE ( 'NONE', #1282, #20006 ) ;
#17370 = VECTOR ( 'NONE', #12043, 1000.000000000000000 ) ;
#17371 = CARTESIAN_POINT ( 'NONE',  ( 3.958484000407108461, 3.734437307742041412, 0.5317648453098983152 ) ) ;
#17372 = CARTESIAN_POINT ( 'NONE',  ( -7.345446946324412529, -0.2181520686730616942, 7.860330092053889217 ) ) ;
#17373 = AXIS2_PLACEMENT_3D ( 'NONE', #18650, #7949, #22305 ) ;
#17374 = VECTOR ( 'NONE', #4380, 1000.000000000000000 ) ;
#17375 = AXIS2_PLACEMENT_3D ( 'NONE', #4786, #4893, #19492 ) ;
#17376 = DIRECTION ( 'NONE',  ( 3.254448077146059901E-32, 1.000000000000000000, 6.409494854920712161E-31 ) ) ;
#17377 = CYLINDRICAL_SURFACE ( 'NONE', #17564, 0.5000000000000038858 ) ;
#17378 = CARTESIAN_POINT ( 'NONE',  ( 0.3126073911695753660, -2.020725942163792421, -3.499999999999996891 ) ) ;
#17379 = CARTESIAN_POINT ( 'NONE',  ( -4.000000000000003553, 2.309401076758494487, -5.600000000000000533 ) ) ;
#17380 = DIRECTION ( 'NONE',  ( 1.000000000000000000, 0.000000000000000000, -0.000000000000000000 ) ) ;
#17381 = ADVANCED_FACE ( 'NONE', ( #18006 ), #18919, .T. ) ;
#17382 = DIRECTION ( 'NONE',  ( -0.000000000000000000, -1.000000000000000000, 0.000000000000000000 ) ) ;
#17383 = ORIENTED_EDGE ( 'NONE', *, *, #17044, .F. ) ;
#17384 = CIRCLE ( 'NONE', #12937, 0.4999999999999990563 ) ;
#17385 = VECTOR ( 'NONE', #20955, 1000.000000000000000 ) ;
#17386 = ORIENTED_EDGE ( 'NONE', *, *, #17211, .F. ) ;
#17387 = AXIS2_PLACEMENT_3D ( 'NONE', #18508, #4821, #6169 ) ;
#17388 = AXIS2_PLACEMENT_3D ( 'NONE', #15782, #3099, #16016 ) ;
#17389 = AXIS2_PLACEMENT_3D ( 'NONE', #6732, #14139, #16119 ) ;
#17390 = CIRCLE ( 'NONE', #6143, 2.550000000000010481 ) ;
#17392 = VERTEX_POINT ( 'NONE', #127 ) ;
#17391 = ORIENTED_EDGE ( 'NONE', *, *, #18713, .F. ) ;
#17393 = EDGE_CURVE ( 'NONE', #6728, #6445, #3968, .T. ) ;
#17394 = CARTESIAN_POINT ( 'NONE',  ( -6.999999999999992006, -8.000000000000044409, 6.250000000000019540 ) ) ;
#17395 = CARTESIAN_POINT ( 'NONE',  ( -4.950765356264206218, 36.36782871084107427, -26.02439111740734035 ) ) ;
#17396 = EDGE_LOOP ( 'NONE', ( #17386, #18418, #20152, #21031, #8588, #21136 ) ) ;
#17397 = CARTESIAN_POINT ( 'NONE',  ( 54.42435809754115894, 0.4999999999999449329, 6.000000000000136779 ) ) ;
#17398 = CARTESIAN_POINT ( 'NONE',  ( 3.806834918298644066, -3.469446951953614189E-14, -3.500000000000012434 ) ) ;
#17399 = DIRECTION ( 'NONE',  ( 9.693522803355793065E-26, -5.963788443470848352E-28, -1.000000000000000000 ) ) ;
#17400 = CARTESIAN_POINT ( 'NONE',  ( 37.52451905283849953, 0.09150635094611496434, -10.18301270189224539 ) ) ;
#17401 = EDGE_CURVE ( 'NONE', #15368, #14653, #5021, .T. ) ;
#17402 = DIRECTION ( 'NONE',  ( 9.693647360340828445E-26, 0.000000000000000000, -1.000000000000000000 ) ) ;
#17403 = CIRCLE ( 'NONE', #15908, 3.499999999999995115 ) ;
#17404 = TOROIDAL_SURFACE ( 'NONE', #5407, 6.500000000000000888, 0.5000000000000000000 ) ;
#17405 = DIRECTION ( 'NONE',  ( 1.000000000000000000, 0.000000000000000000, 0.000000000000000000 ) ) ;
#17406 = CIRCLE ( 'NONE', #6899, 0.5000000000000004441 ) ;
#17407 = FACE_OUTER_BOUND ( 'NONE', #22119, .T. ) ;
#17408 = AXIS2_PLACEMENT_3D ( 'NONE', #19493, #10437, #5385 ) ;
#17409 = CARTESIAN_POINT ( 'NONE',  ( -6.958039891257955745, 36.00029345514013102, -18.49999999999999645 ) ) ;
#17411 = EDGE_CURVE ( 'NONE', #19782, #9536, #18455, .T. ) ;
#17410 = VECTOR ( 'NONE', #17753, 1000.000000000000000 ) ;
#17412 = DIRECTION ( 'NONE',  ( 0.000000000000000000, 0.000000000000000000, 1.000000000000000000 ) ) ;
#17413 = CARTESIAN_POINT ( 'NONE',  ( 4.175075985190096262, -4.120741555260244660, -3.469446951953614189E-15 ) ) ;
#17414 = ORIENTED_EDGE ( 'NONE', *, *, #426, .T. ) ;
#17415 = EDGE_CURVE ( 'NONE', #3554, #20913, #9162, .T. ) ;
#17416 = EDGE_CURVE ( 'NONE', #9299, #18640, #12151, .T. ) ;
#17418 = ORIENTED_EDGE ( 'NONE', *, *, #20471, .F. ) ;
#17417 = ORIENTED_EDGE ( 'NONE', *, *, #5225, .F. ) ;
#17419 = EDGE_CURVE ( 'NONE', #8586, #14201, #5650, .T. ) ;
#17420 = EDGE_LOOP ( 'NONE', ( #2378, #11580, #18276, #7128 ) ) ;
#17421 = VECTOR ( 'NONE', #3478, 1000.000000000000000 ) ;
#17423 = ORIENTED_EDGE ( 'NONE', *, *, #19165, .T. ) ;
#17422 = EDGE_LOOP ( 'NONE', ( #3805, #6726, #20247, #1576 ) ) ;
#17424 = AXIS2_PLACEMENT_3D ( 'NONE', #765, #18751, #7584 ) ;
#17425 = ORIENTED_EDGE ( 'NONE', *, *, #16566, .F. ) ;
#17426 = LINE ( 'NONE', #8496, #6512 ) ;
#17427 = VECTOR ( 'NONE', #12513, 1000.000000000000000 ) ;
#17428 = CARTESIAN_POINT ( 'NONE',  ( -12.84999999999999964, 0.000000000000000000, 0.000000000000000000 ) ) ;
#17429 = DIRECTION ( 'NONE',  ( 0.000000000000000000, -6.938893903907245733E-15, -1.000000000000000000 ) ) ;
#17430 = DIRECTION ( 'NONE',  ( 1.000000000000000000, -4.190823558986610327E-31, 1.733449886265890494E-32 ) ) ;
#17431 = B_SPLINE_CURVE_WITH_KNOTS ( 'NONE', 3,
 ( #3299, #12212, #18103, #10468, #14464, #23183, #19522, #6947 ),
 .UNSPECIFIED., .F., .F.,
 ( 4, 2, 2, 4 ),
 ( 2.465131516947375851E-07, 0.001183067374689833733, 0.001774477805458903349, 0.002365888236227973399 ),
 .UNSPECIFIED. ) ;
#17432 = DIRECTION ( 'NONE',  ( -1.000000000000000000, -2.220446049250307904E-16, 0.000000000000000000 ) ) ;
#17433 = EDGE_CURVE ( 'NONE', #14397, #19077, #9410, .T. ) ;
#17434 = CYLINDRICAL_SURFACE ( 'NONE', #20001, 5.999999999999998224 ) ;
#17435 = EDGE_CURVE ( 'NONE', #2500, #4523, #14418, .T. ) ;
#17436 = ADVANCED_FACE ( 'NONE', ( #18346 ), #10917, .T. ) ;
#17437 = CARTESIAN_POINT ( 'NONE',  ( 25.00000000000001776, 1.250000000000028866, -2.000000000000005329 ) ) ;
#17438 = FACE_OUTER_BOUND ( 'NONE', #11518, .T. ) ;
#17439 = DIRECTION ( 'NONE',  ( -1.000000000000000000, 1.700709290173333260E-16, 0.000000000000000000 ) ) ;
#17440 = DIRECTION ( 'NONE',  ( 0.5000000000000006661, -2.269329254444893839E-16, -0.8660254037844382635 ) ) ;
#17441 = CARTESIAN_POINT ( 'NONE',  ( 0.3126073911696447549, -2.020725942163688504, 3.499999999999997780 ) ) ;
#17442 = AXIS2_PLACEMENT_3D ( 'NONE', #19793, #3674, #17914 ) ;
#17443 = CLOSED_SHELL ( 'NONE', ( #9728, #13298, #18599, #894, #7365, #3369, #4156, #13119, #4053, #785, #8375, #8258, #21890, #16531, #4109, #4236, #5051, #13419, #855, #13765, #4059, #5674, #7875, #17702, #9217, #22912, #11517, #21307, #8846, #11653, #19304, #16502 ) ) ;
#17444 = VECTOR ( 'NONE', #3197, 1000.000000000000000 ) ;
#17445 = DIRECTION ( 'NONE',  ( 3.254448077146059901E-32, 1.000000000000000000, 6.409494854920712161E-31 ) ) ;
#17446 = CARTESIAN_POINT ( 'NONE',  ( 5.051814855409131333, 4.882486540518882201, 6.249999999999979572 ) ) ;
#17447 = EDGE_CURVE ( 'NONE', #690, #13411, #22311, .T. ) ;
#17448 = LINE ( 'NONE', #11080, #6641 ) ;
#17449 = CIRCLE ( 'NONE', #13329, 0.5000000000000009992 ) ;
#17450 = VERTEX_POINT ( 'NONE', #16448 ) ;
#17451 = ADVANCED_FACE ( 'NONE', ( #16675 ), #17404, .T. ) ;
#17453 = ORIENTED_EDGE ( 'NONE', *, *, #15626, .T. ) ;
#17452 = ORIENTED_EDGE ( 'NONE', *, *, #23064, .T. ) ;
#17454 = EDGE_LOOP ( 'NONE', ( #6813, #5633, #14253, #8236 ) ) ;
#17455 = EDGE_LOOP ( 'NONE', ( #20510, #15398, #16599, #5575, #7688, #14856, #14998 ) ) ;
#17456 = ORIENTED_EDGE ( 'NONE', *, *, #19000, .F. ) ;
#17457 = EDGE_LOOP ( 'NONE', ( #5588, #4677, #9596, #7966, #13236, #9589, #17047, #11659, #19808, #8265, #9017, #12416 ) ) ;
#17458 = CARTESIAN_POINT ( 'NONE',  ( 1.199999999999992628, 0.000000000000000000, 0.000000000000000000 ) ) ;
#17459 = AXIS2_PLACEMENT_3D ( 'NONE', #8129, #11765, #20851 ) ;
#17460 = CONICAL_SURFACE ( 'NONE', #10329, 4.750000000000000000, 1.047197551196600074 ) ;
#17461 = B_SPLINE_CURVE_WITH_KNOTS ( 'NONE', 3,
 ( #10756, #3130, #1367, #19711, #23006, #19231 ),
 .UNSPECIFIED., .F., .F.,
 ( 4, 2, 4 ),
 ( 0.004120275011746847918, 0.005288420935197131814, 0.006456566858647415710 ),
 .UNSPECIFIED. ) ;
#17462 = DIRECTION ( 'NONE',  ( 0.000000000000000000, 1.000000000000000000, 0.000000000000000000 ) ) ;
#17463 = ORIENTED_EDGE ( 'NONE', *, *, #7173, .F. ) ;
#17464 = CARTESIAN_POINT ( 'NONE',  ( 3.000000000291852764, 42.99999999900385461, -19.49999999999998934 ) ) ;
#17465 = CARTESIAN_POINT ( 'NONE',  ( 2.678494666091052689, 3.072372537026353267, -5.565789719053469753 ) ) ;
#17466 = FACE_OUTER_BOUND ( 'NONE', #6098, .T. ) ;
#17467 = LINE ( 'NONE', #21127, #5976 ) ;
#17468 = DIRECTION ( 'NONE',  ( 1.000000000000000000, 4.440892098500626162E-16, -5.551115123125782702E-16 ) ) ;
#17469 = CARTESIAN_POINT ( 'NONE',  ( 4.580847626786066940, -1.750000000000001110, 1.565739168675225779 ) ) ;
#17470 = CARTESIAN_POINT ( 'NONE',  ( -2.742413778650712342, -1.325747111984083793, 4.749999999999999112 ) ) ;
#17471 = DIRECTION ( 'NONE',  ( 1.550910762415566494E-16, 1.000000000000000000, -8.135128085091684243E-31 ) ) ;
#17472 = CARTESIAN_POINT ( 'NONE',  ( -6.587771436282949367, 13.98878796535109359, -17.46895447544054747 ) ) ;
#17473 = EDGE_CURVE ( 'NONE', #19925, #8301, #15716, .T. ) ;
#17474 = CARTESIAN_POINT ( 'NONE',  ( -2.428612866367529932E-14, 60.00000000000000000, 6.938893903907228378E-15 ) ) ;
#17475 = VERTEX_POINT ( 'NONE', #585 ) ;
#17476 =( NAMED_UNIT ( * ) PLANE_ANGLE_UNIT ( ) SI_UNIT ( $, .RADIAN. ) );
#17478 = EDGE_CURVE ( 'NONE', #10144, #2826, #7750, .T. ) ;
#17477 = CARTESIAN_POINT ( 'NONE',  ( 4.086262629614028086, 1.979770830881089294, 3.570936333571107735 ) ) ;
#17479 = DIRECTION ( 'NONE',  ( 0.000000000000000000, 0.000000000000000000, 1.000000000000000000 ) ) ;
#17481 = EDGE_LOOP ( 'NONE', ( #3239, #22436, #15421 ) ) ;
#17480 = ORIENTED_EDGE ( 'NONE', *, *, #9374, .T. ) ;
#17482 = EDGE_CURVE ( 'NONE', #8658, #343, #14024, .T. ) ;
#17483 = VERTEX_POINT ( 'NONE', #13049 ) ;
#17484 = ORIENTED_EDGE ( 'NONE', *, *, #13980, .T. ) ;
#17485 = CARTESIAN_POINT ( 'NONE',  ( 4.082498951862915781, 2.020725942163688504, 3.499999999999997780 ) ) ;
#17486 = DIRECTION ( 'NONE',  ( 4.190823558986625216E-31, -1.000000000000000000, 4.190823558986625216E-31 ) ) ;
#17487 = AXIS2_PLACEMENT_3D ( 'NONE', #1084, #6800, #17618 ) ;
#17488 = CARTESIAN_POINT ( 'NONE',  ( 30.15500000000000114, 8.245366548881241351E-15, -2.500000000000023093 ) ) ;
#17489 = CARTESIAN_POINT ( 'NONE',  ( 3.961551342853960378, 3.742715940867782365, -0.5174258321190572385 ) ) ;
#17490 = CARTESIAN_POINT ( 'NONE',  ( -12.84999999999999964, -13.50000000000011191, -5.749999999999949374 ) ) ;
#17491 =( GEOMETRIC_REPRESENTATION_CONTEXT ( 3 ) GLOBAL_UNCERTAINTY_ASSIGNED_CONTEXT ( ( #7685 ) ) GLOBAL_UNIT_ASSIGNED_CONTEXT ( ( #3474, #10759, #16160 ) ) REPRESENTATION_CONTEXT ( 'NONE', 'WORKASPACE' ) );
#17492 = DIRECTION ( 'NONE',  ( 1.000000000000000000, 3.026128730315075503E-14, 0.000000000000000000 ) ) ;
#17493 = FACE_OUTER_BOUND ( 'NONE', #19835, .T. ) ;
#17494 = APPLICATION_CONTEXT ( 'automotive_design' ) ;
#17495 = CARTESIAN_POINT ( 'NONE',  ( -7.604097569491801600, -0.4107518873689900429, 8.440516644273033720 ) ) ;
#17496 = DIRECTION ( 'NONE',  ( -0.000000000000000000, -0.000000000000000000, 1.000000000000000000 ) ) ;
#17497 = DIRECTION ( 'NONE',  ( -1.000000000000000000, -2.699383410053119644E-30, -3.330669073875432643E-16 ) ) ;
#17498 = TOROIDAL_SURFACE ( 'NONE', #23150, 5.750000000000000000, 0.5000000000000000000 ) ;
#17499 = FACE_OUTER_BOUND ( 'NONE', #3203, .T. ) ;
#17500 = DIRECTION ( 'NONE',  ( 0.3420201433256618850, 1.150791560227853967E-16, 0.9396926207859108704 ) ) ;
#17501 = CARTESIAN_POINT ( 'NONE',  ( 1.200000000000006617, 0.5999999999999998668, -4.749999999999948486 ) ) ;
#17502 = VECTOR ( 'NONE', #21050, 999.9999999999998863 ) ;
#17503 = DIRECTION ( 'NONE',  ( -1.066786462891689527E-26, -6.656013887802287108E-31, -1.000000000000000000 ) ) ;
#17504 = ORIENTED_EDGE ( 'NONE', *, *, #3827, .F. ) ;
#17505 = CIRCLE ( 'NONE', #10374, 0.5000000000000038858 ) ;
#17506 = EDGE_LOOP ( 'NONE', ( #13655, #8008, #16943, #20679 ) ) ;
#17507 = DIRECTION ( 'NONE',  ( 0.000000000000000000, -3.382522293539642133E-32, -1.000000000000000000 ) ) ;
#17509 = ORIENTED_EDGE ( 'NONE', *, *, #23005, .F. ) ;
#17508 = ORIENTED_EDGE ( 'NONE', *, *, #11822, .F. ) ;
#17510 = VECTOR ( 'NONE', #21295, 1000.000000000000000 ) ;
#17511 = CARTESIAN_POINT ( 'NONE',  ( -3.997250504095275048, -1.750000000000057288, -2.576559036326496965 ) ) ;
#17512 = ORIENTED_EDGE ( 'NONE', *, *, #21013, .F. ) ;
#17513 = SURFACE_SIDE_STYLE ('',( #19397 ) ) ;
#17514 = CIRCLE ( 'NONE', #17140, 0.5000000000000029976 ) ;
#17515 = EDGE_CURVE ( 'NONE', #6309, #5339, #14808, .T. ) ;
#17516 = DIRECTION ( 'NONE',  ( 1.000000000000000000, 2.282530889443153710E-16, 8.673617379883983210E-16 ) ) ;
#17517 = ORIENTED_EDGE ( 'NONE', *, *, #4901, .T. ) ;
#17518 = DIRECTION ( 'NONE',  ( 0.000000000000000000, 0.000000000000000000, -1.000000000000000000 ) ) ;
#17519 = LINE ( 'NONE', #23073, #14934 ) ;
#17520 = AXIS2_PLACEMENT_3D ( 'NONE', #18150, #5907, #5685 ) ;
#17521 = FACE_OUTER_BOUND ( 'NONE', #6474, .T. ) ;
#17522 = DIRECTION ( 'NONE',  ( -0.000000000000000000, 1.000000000000000000, -0.000000000000000000 ) ) ;
#17523 = DIRECTION ( 'NONE',  ( -1.000000000000000000, 1.065615849528602702E-14, 0.000000000000000000 ) ) ;
#17524 = CARTESIAN_POINT ( 'NONE',  ( -3.344563996438217224, -2.687817229851500400, -5.441324518471499339 ) ) ;
#17525 = CARTESIAN_POINT ( 'NONE',  ( 22.49999999999998224, 2.000000000000001776, -0.2500000000000210387 ) ) ;
#17526 = SURFACE_STYLE_USAGE ( .BOTH. , #10355 ) ;
#17527 = VECTOR ( 'NONE', #6681, 1000.000000000000000 ) ;
#17528 = PLANE ( 'NONE',  #7829 ) ;
#17529 = CARTESIAN_POINT ( 'NONE',  ( 4.158413352280815545, -4.089743253945648860, 1.734723475976807094E-15 ) ) ;
#17530 = VERTEX_POINT ( 'NONE', #12700 ) ;
#17531 = AXIS2_PLACEMENT_3D ( 'NONE', #6383, #6810, #9784 ) ;
#17532 = DIRECTION ( 'NONE',  ( 0.000000000000000000, 0.000000000000000000, 1.000000000000000000 ) ) ;
#17534 = ORIENTED_EDGE ( 'NONE', *, *, #10358, .T. ) ;
#17533 = ORIENTED_EDGE ( 'NONE', *, *, #11105, .T. ) ;
#17535 = ORIENTED_EDGE ( 'NONE', *, *, #19668, .T. ) ;
#17536 = EDGE_CURVE ( 'NONE', #4283, #22262, #9528, .T. ) ;
#17537 = AXIS2_PLACEMENT_3D ( 'NONE', #12559, #5278, #19748 ) ;
#17539 = VERTEX_POINT ( 'NONE', #22895 ) ;
#17538 = ORIENTED_EDGE ( 'NONE', *, *, #14683, .T. ) ;
#17540 = CARTESIAN_POINT ( 'NONE',  ( 4.050536630291722062, 3.778525289263191311, 0.5912575323400045546 ) ) ;
#17541 = CARTESIAN_POINT ( 'NONE',  ( 1.167157674106084754E-15, 59.74999999999991473, -4.499999999999978684 ) ) ;
#17542 = ADVANCED_FACE ( 'NONE', ( #4447 ), #1369, .T. ) ;
#17543 = DIRECTION ( 'NONE',  ( 1.000000000000000000, 2.664535259100391869E-15, 0.000000000000000000 ) ) ;
#17544 = DIRECTION ( 'NONE',  ( 1.000000000000000000, -4.190823558986610327E-31, 1.733449886265890494E-32 ) ) ;
#17545 = AXIS2_PLACEMENT_3D ( 'NONE', #8458, #20700, #4803 ) ;
#17546 = CARTESIAN_POINT ( 'NONE',  ( -25.39999999999989200, 2.806173731541575138E-14, -2.499999999999920952 ) ) ;
#17547 = CARTESIAN_POINT ( 'NONE',  ( 2.339468227445713033, 3.268109542640643905, 2.462324777668250297E-15 ) ) ;
#17548 = AXIS2_PLACEMENT_3D ( 'NONE', #799, #9617, #9271 ) ;
#17549 = DIRECTION ( 'NONE',  ( -0.7071067811865535679, 0.7071067811865414665, 0.000000000000000000 ) ) ;
#17550 = ADVANCED_FACE ( 'NONE', ( #8102 ), #7646, .T. ) ;
#17551 = CARTESIAN_POINT ( 'NONE',  ( -57.28378781035998912, -0.5000000000000281997, 8.541666666666767327 ) ) ;
#17552 = ADVANCED_FACE ( 'NONE', ( #4324 ), #8032, .T. ) ;
#17553 = DIRECTION ( 'NONE',  ( 1.000000000000000000, -4.190823558986610327E-31, 1.733449886265890494E-32 ) ) ;
#17554 = DIRECTION ( 'NONE',  ( -1.000000000000000000, 0.000000000000000000, 0.000000000000000000 ) ) ;
#17555 = EDGE_CURVE ( 'NONE', #18733, #16673, #10529, .T. ) ;
#17556 = CARTESIAN_POINT ( 'NONE',  ( -6.000000000000074607, -7.500000000000027534, -7.500000000000034639 ) ) ;
#17557 = AXIS2_PLACEMENT_3D ( 'NONE', #22136, #12971, #7901 ) ;
#17558 = CARTESIAN_POINT ( 'NONE',  ( -3.499999999708153453, 35.99999999900384751, -19.00000000000000355 ) ) ;
#17559 = CARTESIAN_POINT ( 'NONE',  ( 12.84999999999997300, -12.00000000000006928, 4.163336342344337027E-14 ) ) ;
#17560 = DIRECTION ( 'NONE',  ( 0.9878135252003127365, 2.193386639427060722E-16, -0.1556420233463029767 ) ) ;
#17561 = PRODUCT_DEFINITION_SHAPE ( 'NONE', 'NONE',  #23278 ) ;
#17562 = AXIS2_PLACEMENT_3D ( 'NONE', #767, #14524, #415 ) ;
#17563 = ORIENTED_EDGE ( 'NONE', *, *, #594, .T. ) ;
#17564 = AXIS2_PLACEMENT_3D ( 'NONE', #22810, #17497, #1288 ) ;
#17566 = EDGE_LOOP ( 'NONE', ( #3578, #16728, #8441, #8446 ) ) ;
#17565 = ORIENTED_EDGE ( 'NONE', *, *, #20002, .T. ) ;
#17567 = EDGE_CURVE ( 'NONE', #20156, #1550, #13938, .T. ) ;
#17568 = CIRCLE ( 'NONE', #17193, 0.5000000000000014433 ) ;
#17569 = EDGE_LOOP ( 'NONE', ( #12080, #111, #247, #20506, #2622, #13924 ) ) ;
#17570 = EDGE_CURVE ( 'NONE', #21116, #16513, #5120, .T. ) ;
#17571 = ORIENTED_EDGE ( 'NONE', *, *, #9598, .F. ) ;
#17572 = AXIS2_PLACEMENT_3D ( 'NONE', #5877, #18680, #3863 ) ;
#17573 = ORIENTED_EDGE ( 'NONE', *, *, #4488, .T. ) ;
#17574 = VERTEX_POINT ( 'NONE', #15808 ) ;
#17575 = CARTESIAN_POINT ( 'NONE',  ( 24.75000000000002487, 1.250000000000001110, -2.081668171172168513E-14 ) ) ;
#17576 = CIRCLE ( 'NONE', #310, 5.500000000000032863 ) ;
#17577 = DIRECTION ( 'NONE',  ( -0.7071067811865507924, -0.7071067811865444641, -2.121016688166342479E-16 ) ) ;
#17578 = EDGE_CURVE ( 'NONE', #21118, #18025, #8536, .T. ) ;
#17579 = ORIENTED_EDGE ( 'NONE', *, *, #183, .T. ) ;
#17580 = DIRECTION ( 'NONE',  ( -0.7071067811865490160, -0.7071067811865460184, -1.565905175853766674E-16 ) ) ;
#17581 = CARTESIAN_POINT ( 'NONE',  ( -6.999999999708156118, 6.999999999003851947, -19.00000000000000355 ) ) ;
#17582 = EDGE_CURVE ( 'NONE', #6218, #5465, #9558, .T. ) ;
#17583 = CARTESIAN_POINT ( 'NONE',  ( 25.60000000000000142, 0.000000000000000000, -6.938893903907228378E-15 ) ) ;
#17584 = DIRECTION ( 'NONE',  ( -1.000000000000000000, 0.000000000000000000, 0.000000000000000000 ) ) ;
#17585 = DIRECTION ( 'NONE',  ( -3.330669073875432643E-16, -4.437342591868153746E-31, 1.000000000000000000 ) ) ;
#17586 = DIRECTION ( 'NONE',  ( -2.172745813409349776E-17, 1.000000000000000000, -1.309377075419428048E-16 ) ) ;
#17587 = CARTESIAN_POINT ( 'NONE',  ( -2.296348136192885026, -1.454515171358716552, 4.749999999999999112 ) ) ;
#17588 = ADVANCED_FACE ( 'NONE', ( #4997 ), #1588, .F. ) ;
#17589 = AXIS2_PLACEMENT_3D ( 'NONE', #850, #8022, #20731 ) ;
#17590 = DIRECTION ( 'NONE',  ( 1.000000000000000000, 1.479114197289387852E-30, -2.013525853228518840E-32 ) ) ;
#17591 = DIRECTION ( 'NONE',  ( -1.333893503340774882E-15, -2.778352770573747380E-17, -1.000000000000000000 ) ) ;
#17592 = DIRECTION ( 'NONE',  ( 1.000000000000000000, 1.479114197289388027E-30, -2.013525853228518840E-32 ) ) ;
#17593 = VECTOR ( 'NONE', #19740, 1000.000000000000000 ) ;
#17594 = DIRECTION ( 'NONE',  ( 0.000000000000000000, -1.000000000000000000, 0.000000000000000000 ) ) ;
#17595 = EDGE_LOOP ( 'NONE', ( #8664, #2647, #23129, #2379, #8516, #12266, #8213, #10166, #15135, #7172, #3026, #22615, #65 ) ) ;
#17596 = CIRCLE ( 'NONE', #21383, 2.250000000000001776 ) ;
#17597 = SURFACE_SIDE_STYLE ('',( #5008 ) ) ;
#17598 = CARTESIAN_POINT ( 'NONE',  ( 26.09619407800441948, 29.09619407671641866, -26.00000000000000000 ) ) ;
#17599 = CIRCLE ( 'NONE', #5196, 0.2500000000000000000 ) ;
#17600 = DIRECTION ( 'NONE',  ( -1.000000000000000000, -2.699383410053119644E-30, -3.330669073875432643E-16 ) ) ;
#17601 = CIRCLE ( 'NONE', #4445, 1.300000000000009592 ) ;
#17603 = ORIENTED_EDGE ( 'NONE', *, *, #8224, .F. ) ;
#17602 = ORIENTED_EDGE ( 'NONE', *, *, #14532, .F. ) ;
#17604 = EDGE_CURVE ( 'NONE', #2357, #15246, #16643, .T. ) ;
#17605 = ORIENTED_EDGE ( 'NONE', *, *, #3258, .T. ) ;
#17606 = ORIENTED_EDGE ( 'NONE', *, *, #10575, .F. ) ;
#17607 = DIRECTION ( 'NONE',  ( 2.013525853228507892E-32, 6.902532920683810383E-31, -1.000000000000000000 ) ) ;
#17608 = CARTESIAN_POINT ( 'NONE',  ( -45.37157287525420202, 6.828427124746169419, 7.500000000000089706 ) ) ;
#17609 = CARTESIAN_POINT ( 'NONE',  ( -2.000000000000015543, 3.464101615137746837, 0.000000000000000000 ) ) ;
#17610 = EDGE_CURVE ( 'NONE', #9040, #20589, #7289, .T. ) ;
#17611 = CARTESIAN_POINT ( 'NONE',  ( 63.53596085922837489, -4.500000000000059508, -6.499999999999957367 ) ) ;
#17612 = DIRECTION ( 'NONE',  ( 0.9706398123736329486, 2.155253336630096955E-16, 0.2405376366294442458 ) ) ;
#17613 = CIRCLE ( 'NONE', #15740, 0.5000000000000038858 ) ;
#17614 = LINE ( 'NONE', #1506, #4575 ) ;
#17615 = CARTESIAN_POINT ( 'NONE',  ( 30.60000000000000142, 2.775557561562891351E-14, -2.081668171172168513E-14 ) ) ;
#17616 = TOROIDAL_SURFACE ( 'NONE', #13124, 2.500000000000002220, 0.5000000000000000000 ) ;
#17617 = DIRECTION ( 'NONE',  ( -1.000000000000000000, 3.742046355321372466E-14, 0.000000000000000000 ) ) ;
#17618 = DIRECTION ( 'NONE',  ( -1.000000000000000000, 0.000000000000000000, -8.438582421954110511E-32 ) ) ;
#17619 = CARTESIAN_POINT ( 'NONE',  ( 110.9706201109471522, -9.453020409440265226, 6.500000000000095923 ) ) ;
#17620 = CARTESIAN_POINT ( 'NONE',  ( 37.86602540378468262, 11.00000000000000533, -10.86602540378449255 ) ) ;
#17621 = DIRECTION ( 'NONE',  ( 1.000000000000000000, 0.000000000000000000, 0.000000000000000000 ) ) ;
#17622 = LINE ( 'NONE', #17865, #19060 ) ;
#17623 = DIRECTION ( 'NONE',  ( -1.000000000000000000, 4.190823558986610327E-31, -1.733449886265890494E-32 ) ) ;
#17624 = DIRECTION ( 'NONE',  ( 1.066788928082016908E-26, -6.656013887802287108E-31, -1.000000000000000000 ) ) ;
#17625 = DIRECTION ( 'NONE',  ( 0.4472135954999587604, 0.7745966692414837373, 0.4472135954999567620 ) ) ;
#17626 = VERTEX_POINT ( 'NONE', #3252 ) ;
#17627 = AXIS2_PLACEMENT_3D ( 'NONE', #10907, #113, #11265 ) ;
#17628 = ORIENTED_EDGE ( 'NONE', *, *, #14153, .T. ) ;
#17629 = FACE_OUTER_BOUND ( 'NONE', #19129, .T. ) ;
#17631 = ORIENTED_EDGE ( 'NONE', *, *, #22479, .T. ) ;
#17630 = ORIENTED_EDGE ( 'NONE', *, *, #16826, .F. ) ;
#17632 = DIRECTION ( 'NONE',  ( 2.172745813409349776E-17, -1.000000000000000000, 1.309377075419428048E-16 ) ) ;
#17633 = EDGE_CURVE ( 'NONE', #16351, #13358, #2009, .T. ) ;
#17634 = EDGE_LOOP ( 'NONE', ( #147, #11813, #20964, #18642 ) ) ;
#17635 = CARTESIAN_POINT ( 'NONE',  ( -45.56568542494951402, 2.108831175456883589, 8.000000000000035527 ) ) ;
#17636 = PRODUCT_DEFINITION_FORMATION_WITH_SPECIFIED_SOURCE ( 'ANY', '', #7073, .NOT_KNOWN. ) ;
#17637 = CARTESIAN_POINT ( 'NONE',  ( -5.197224361976157780, 36.49999999900384751, -19.00000000000000355 ) ) ;
#17638 = VERTEX_POINT ( 'NONE', #6228 ) ;
#17639 = CARTESIAN_POINT ( 'NONE',  ( 25.00000000000000355, 2.000000000000001776, -2.000000000000005329 ) ) ;
#17640 = DIRECTION ( 'NONE',  ( 3.885780586188016830E-16, 4.437342591868156373E-31, -1.000000000000000000 ) ) ;
#17641 = DIRECTION ( 'NONE',  ( 1.066786462891689527E-26, 6.656013887802287108E-31, 1.000000000000000000 ) ) ;
#17642 = ADVANCED_FACE ( 'NONE', ( #11620 ), #18809, .T. ) ;
#17643 = CARTESIAN_POINT ( 'NONE',  ( -7.168696526429614302, -13.62622308581068253, 8.340670630249134021 ) ) ;
#17644 = CARTESIAN_POINT ( 'NONE',  ( 4.050480423730739687, 1.376911654797406515, -3.567926555162024282 ) ) ;
#17645 = CARTESIAN_POINT ( 'NONE',  ( 4.175813232069149450, 2.061359961916364725, -3.570380186727398986 ) ) ;
#17646 = CARTESIAN_POINT ( 'NONE',  ( 2.775557561562891351E-14, 2.999999999999999112, -12.99999999999999822 ) ) ;
#17647 =( NAMED_UNIT ( * ) SI_UNIT ( $, .STERADIAN. ) SOLID_ANGLE_UNIT ( ) );
#17648 =( LENGTH_UNIT ( ) NAMED_UNIT ( * ) SI_UNIT ( .MILLI., .METRE. ) );
#17649 =( LENGTH_UNIT ( ) NAMED_UNIT ( * ) SI_UNIT ( .MILLI., .METRE. ) );
#17650 = CARTESIAN_POINT ( 'NONE',  ( 0.000000000000000000, 3.031088913245536087, 1.750000000000003331 ) ) ;
#17651 = ORIENTED_EDGE ( 'NONE', *, *, #7216, .T. ) ;
#17652 = CARTESIAN_POINT ( 'NONE',  ( -56.82380924748794371, 68.02044774975502150, 24.66570243528390094 ) ) ;
#17654 = ORIENTED_EDGE ( 'NONE', *, *, #14979, .T. ) ;
#17653 = ORIENTED_EDGE ( 'NONE', *, *, #13262, .T. ) ;
#17655 = B_SPLINE_CURVE_WITH_KNOTS ( 'NONE', 3,
 ( #19874, #16329, #1752, #12452 ),
 .UNSPECIFIED., .F., .F.,
 ( 4, 4 ),
 ( 2.380739281923877002E-07, 0.002044882221487566605 ),
 .UNSPECIFIED. ) ;
#17656 = ORIENTED_EDGE ( 'NONE', *, *, #22019, .T. ) ;
#17658 = VERTEX_POINT ( 'NONE', #12519 ) ;
#17657 = ORIENTED_EDGE ( 'NONE', *, *, #5862, .T. ) ;
#17659 = DIRECTION ( 'NONE',  ( -1.000000000000000000, -1.910522504832140594E-31, 5.551115123125818447E-17 ) ) ;
#17660 = DIRECTION ( 'NONE',  ( -1.000000000000000000, -2.699383410053119644E-30, -3.330669073875432643E-16 ) ) ;
#17661 = DIRECTION ( 'NONE',  ( -1.000000000000000000, -2.699383410053119644E-30, -3.330669073875432643E-16 ) ) ;
#17662 = PLANE ( 'NONE',  #4562 ) ;
#17663 = VECTOR ( 'NONE', #23218, 1000.000000000000000 ) ;
#17664 = CARTESIAN_POINT ( 'NONE',  ( 4.330127018922110160, -5.551115123125782702E-14, -7.499999999999996447 ) ) ;
#17665 = DIRECTION ( 'NONE',  ( -1.000000000000000000, 4.190823558986610327E-31, -1.733449886265890494E-32 ) ) ;
#17666 = CARTESIAN_POINT ( 'NONE',  ( -90.63385214007838897, -7.632783294297951215E-14, -7.926881151201908615 ) ) ;
#17667 = DIRECTION ( 'NONE',  ( -1.000000000000000000, 4.625929269271439095E-14, -3.854941057726199147E-16 ) ) ;
#17668 = DIRECTION ( 'NONE',  ( 6.409494854920715664E-31, 0.8660254037844388186, 0.4999999999999997224 ) ) ;
#17669 = CARTESIAN_POINT ( 'NONE',  ( 0.000000000000000000, 0.000000000000000000, -5.600000000000000533 ) ) ;
#17670 = CARTESIAN_POINT ( 'NONE',  ( -1.387778780781445676E-14, -24.99999999999998224, 0.000000000000000000 ) ) ;
#17671 = FACE_OUTER_BOUND ( 'NONE', #16863, .T. ) ;
#17672 = PRODUCT_DEFINITION ( 'UNKNOWN', '', #17636, #2995 ) ;
#17673 = LINE ( 'NONE', #5222, #10797 ) ;
#17674 = CARTESIAN_POINT ( 'NONE',  ( -2.700000000000035705, 7.199999999999977085, -7.500000000000007105 ) ) ;
#17675 = DIRECTION ( 'NONE',  ( 2.013525853228507892E-32, 6.902532920683810383E-31, -1.000000000000000000 ) ) ;
#17676 = CARTESIAN_POINT ( 'NONE',  ( -55.05572809000122447, -2.700000000000125855, -10.00000000000006395 ) ) ;
#17677 = ORIENTED_EDGE ( 'NONE', *, *, #4713, .T. ) ;
#17678 = EDGE_CURVE ( 'NONE', #22641, #15514, #3638, .T. ) ;
#17679 = VERTEX_POINT ( 'NONE', #190 ) ;
#17680 =( NAMED_UNIT ( * ) PLANE_ANGLE_UNIT ( ) SI_UNIT ( $, .RADIAN. ) );
#17681 = AXIS2_PLACEMENT_3D ( 'NONE', #18601, #2591, #4470 ) ;
#17683 = VERTEX_POINT ( 'NONE', #14415 ) ;
#17682 = ORIENTED_EDGE ( 'NONE', *, *, #7805, .F. ) ;
#17684 = ORIENTED_EDGE ( 'NONE', *, *, #11622, .F. ) ;
#17685 = EDGE_CURVE ( 'NONE', #7941, #20683, #16281, .T. ) ;
#17686 = ORIENTED_EDGE ( 'NONE', *, *, #18864, .T. ) ;
#17687 = VERTEX_POINT ( 'NONE', #7018 ) ;
#17688 = ORIENTED_EDGE ( 'NONE', *, *, #18745, .T. ) ;
#17689 = CYLINDRICAL_SURFACE ( 'NONE', #18205, 7.000000000000006217 ) ;
#17690 = CARTESIAN_POINT ( 'NONE',  ( -2.306216605489283533E-14, -0.3420925509533392916, 3.499999999999959588 ) ) ;
#17691 = EDGE_CURVE ( 'NONE', #7127, #20569, #6159, .T. ) ;
#17692 = VERTEX_POINT ( 'NONE', #3932 ) ;
#17693 = DIRECTION ( 'NONE',  ( -2.220446049250313081E-16, 1.000000000000000000, -7.025792437124636392E-31 ) ) ;
#17694 = LINE ( 'NONE', #19708, #8367 ) ;
#17695 = LINE ( 'NONE', #7138, #12889 ) ;
#17696 = CARTESIAN_POINT ( 'NONE',  ( -50.65685424949280247, 2.700000000000021938, 8.000000000000090594 ) ) ;
#17697 = AXIS2_PLACEMENT_3D ( 'NONE', #6799, #17259, #3042 ) ;
#17698 = CIRCLE ( 'NONE', #3065, 0.4999999999999987232 ) ;
#17699 = CARTESIAN_POINT ( 'NONE',  ( 12.49999999999992362, 1.250000000000015099, -4.750000000000000888 ) ) ;
#17700 = CARTESIAN_POINT ( 'NONE',  ( 0.2499999999999828748, 0.2500000000000418554, -17.00000000000000711 ) ) ;
#17701 = FACE_OUTER_BOUND ( 'NONE', #1493, .T. ) ;
#17702 = ADVANCED_FACE ( 'NONE', ( #21374 ), #9262, .F. ) ;
#17703 = DIRECTION ( 'NONE',  ( 0.7071067811865517916, 0.7071067811865431318, 4.556821512286124754E-17 ) ) ;
#17704 = CARTESIAN_POINT ( 'NONE',  ( 37.52451905283849953, 10.90849364905388441, -10.18301270189226315 ) ) ;
#17705 = DIRECTION ( 'NONE',  ( -2.013525853228507892E-32, -6.902532920683810383E-31, 1.000000000000000000 ) ) ;
#17706 = CARTESIAN_POINT ( 'NONE',  ( 30.00000000029184832, -0.5000000009961480529, -39.00000000000000000 ) ) ;
#17707 = ORIENTED_EDGE ( 'NONE', *, *, #6119, .T. ) ;
#17708 = ADVANCED_FACE ( 'NONE', ( #7357 ), #5478, .T. ) ;
#17709 = DIRECTION ( 'NONE',  ( 3.330669073875432643E-16, 4.437342591868153746E-31, -1.000000000000000000 ) ) ;
#17710 = CARTESIAN_POINT ( 'NONE',  ( -55.05572809000125289, 1.387778780781445676E-14, -10.00000000000006395 ) ) ;
#17712 = ORIENTED_EDGE ( 'NONE', *, *, #22928, .F. ) ;
#17711 = ORIENTED_EDGE ( 'NONE', *, *, #10792, .F. ) ;
#17713 = EDGE_CURVE ( 'NONE', #3480, #19838, #9116, .T. ) ;
#17714 = ORIENTED_EDGE ( 'NONE', *, *, #22576, .F. ) ;
#17715 = AXIS2_PLACEMENT_3D ( 'NONE', #17700, #20138, #5250 ) ;
#17716 = AXIS2_PLACEMENT_3D ( 'NONE', #12798, #2214, #11371 ) ;
#17717 = EDGE_CURVE ( 'NONE', #15911, #16493, #3813, .T. ) ;
#17718 = B_SPLINE_CURVE_WITH_KNOTS ( 'NONE', 3,
 ( #1443, #8857, #5323, #10606, #16013, #17912, #14030, #43, #3564, #10726, #9077, #8618, #1788, #21569 ),
 .UNSPECIFIED., .F., .F.,
 ( 4, 2, 2, 2, 2, 2, 4 ),
 ( 1.176546704354857500E-17, 0.0008155857435326490431, 0.001223378615298965216, 0.001631171487065281823, 0.002038964358831596695, 0.002446757230597911784, 0.003262342974130545432 ),
 .UNSPECIFIED. ) ;
#17719 = ORIENTED_EDGE ( 'NONE', *, *, #21026, .F. ) ;
#17720 = EDGE_CURVE ( 'NONE', #11726, #11691, #8774, .T. ) ;
#17721 = ORIENTED_EDGE ( 'NONE', *, *, #1374, .T. ) ;
#17722 = CARTESIAN_POINT ( 'NONE',  ( 42.00000000000014921, 5.500000000000001776, 2.500000000000030198 ) ) ;
#17723 = CYLINDRICAL_SURFACE ( 'NONE', #4204, 0.4999999999999978351 ) ;
#17724 = CARTESIAN_POINT ( 'NONE',  ( -4.580847626786052729, 1.750000000000008438, 1.565739168675228221 ) ) ;
#17725 = CARTESIAN_POINT ( 'NONE',  ( -3.111695183146366136E-17, 6.219541108242305968E-16, 4.750000000000000000 ) ) ;
#17726 = DIRECTION ( 'NONE',  ( 1.000000000000000000, -2.168404344971005170E-16, 1.203141491611682442E-30 ) ) ;
#17727 = CARTESIAN_POINT ( 'NONE',  ( 5.599999999999994316, 0.000000000000000000, 0.000000000000000000 ) ) ;
#17728 = CYLINDRICAL_SURFACE ( 'NONE', #9069, 2.999999999999995559 ) ;
#17729 = CARTESIAN_POINT ( 'NONE',  ( -3.499999999708153453, 13.99999999900385106, -19.50000000000000355 ) ) ;
#17730 = ADVANCED_FACE ( 'NONE', ( #3473 ), #11768, .T. ) ;
#17731 = EDGE_CURVE ( 'NONE', #16744, #10365, #14779, .T. ) ;
#17732 = CARTESIAN_POINT ( 'NONE',  ( 0.000000000000000000, 0.000000000000000000, 0.000000000000000000 ) ) ;
#17733 = EDGE_CURVE ( 'NONE', #15514, #6911, #6188, .T. ) ;
#17734 = DIRECTION ( 'NONE',  ( 2.775557561562883955E-17, -3.406761633869148333E-16, 1.000000000000000000 ) ) ;
#17735 = VECTOR ( 'NONE', #2253, 1000.000000000000000 ) ;
#17736 = VECTOR ( 'NONE', #10321, 1000.000000000000000 ) ;
#17737 = CARTESIAN_POINT ( 'NONE',  ( 2.918498775983380256E-10, 2.999999999003851503, -39.00000000000000000 ) ) ;
#17738 = DIRECTION ( 'NONE',  ( 1.000000000000000000, 2.168404344970992105E-16, 1.734723475976793684E-15 ) ) ;
#17739 = FILL_AREA_STYLE_COLOUR ( '', #9251 ) ;
#17740 = CIRCLE ( 'NONE', #7985, 2.550000000000000711 ) ;
#17741 = DIRECTION ( 'NONE',  ( -0.6819983600624998088, 0.7313537016191693496, 0.000000000000000000 ) ) ;
#17742 = DIRECTION ( 'NONE',  ( -0.8660254037844395958, 0.4999999999999985567, 0.000000000000000000 ) ) ;
#17743 = ORIENTED_EDGE ( 'NONE', *, *, #3231, .F. ) ;
#17744 = EDGE_CURVE ( 'NONE', #7941, #14364, #14872, .T. ) ;
#17745 = ADVANCED_FACE ( 'NONE', ( #875 ), #9179, .T. ) ;
#17746 = TOROIDAL_SURFACE ( 'NONE', #12082, 0.7500000000000000000, 0.2500000000000000000 ) ;
#17747 = ORIENTED_EDGE ( 'NONE', *, *, #1455, .T. ) ;
#17748 = EDGE_CURVE ( 'NONE', #15946, #23148, #4270, .T. ) ;
#17749 = FACE_OUTER_BOUND ( 'NONE', #5110, .T. ) ;
#17751 = ORIENTED_EDGE ( 'NONE', *, *, #2359, .F. ) ;
#17750 = VERTEX_POINT ( 'NONE', #11329 ) ;
#17752 = AXIS2_PLACEMENT_3D ( 'NONE', #21598, #14517, #21707 ) ;
#17753 = DIRECTION ( 'NONE',  ( 5.551115123125761132E-17, -1.577721810442025713E-30, 1.000000000000000000 ) ) ;
#17754 = AXIS2_PLACEMENT_3D ( 'NONE', #18421, #14539, #21963 ) ;
#17755 = CIRCLE ( 'NONE', #5757, 0.2500000000000000000 ) ;
#17756 = CARTESIAN_POINT ( 'NONE',  ( -89.70000000000057128, -9.020562075079396891E-14, -2.000000000000001776 ) ) ;
#17757 = CARTESIAN_POINT ( 'NONE',  ( 2.775557561562891351E-14, 0.2500000000000002220, -6.499999999999950262 ) ) ;
#17758 = AXIS2_PLACEMENT_3D ( 'NONE', #13268, #693, #2673 ) ;
#17759 = LINE ( 'NONE', #3860, #13513 ) ;
#17760 = ORIENTED_EDGE ( 'NONE', *, *, #16541, .F. ) ;
#17761 = CARTESIAN_POINT ( 'NONE',  ( -12.85000000000002807, -1.999999999999998224, 6.249999999999950262 ) ) ;
#17762 = PLANE ( 'NONE',  #16422 ) ;
#17763 = FACE_OUTER_BOUND ( 'NONE', #6564, .T. ) ;
#17764 = PRODUCT_DEFINITION_SHAPE ( 'NONE', 'NONE',  #21145 ) ;
#17765 = CARTESIAN_POINT ( 'NONE',  ( 4.000000000000003553, -0.7779732554280851531, -0.03354435108168089819 ) ) ;
#17766 = CARTESIAN_POINT ( 'NONE',  ( -3.999999999708153453, 35.49999999900384751, -19.50000000000000355 ) ) ;
#17767 = DIRECTION ( 'NONE',  ( 2.013525853228507892E-32, 6.902532920683810383E-31, -1.000000000000000000 ) ) ;
#17768 = CARTESIAN_POINT ( 'NONE',  ( 3.999999999999960032, -2.309401076758530902, -3.504271511726785082 ) ) ;
#17769 = CARTESIAN_POINT ( 'NONE',  ( 37.86602540378461157, 11.00000000000000000, -2.133974596215532316 ) ) ;
#17770 = CARTESIAN_POINT ( 'NONE',  ( 3.999999999999948042, 2.309401076758532678, -5.000000000000000888 ) ) ;
#17771 = CIRCLE ( 'NONE', #19653, 6.500000000000075495 ) ;
#17772 = CARTESIAN_POINT ( 'NONE',  ( -55.25320565519152893, 2.700000000000104983, 8.000000000000035527 ) ) ;
#17773 = AXIS2_PLACEMENT_3D ( 'NONE', #493, #2124, #4346 ) ;
#17774 =( NAMED_UNIT ( * ) SI_UNIT ( $, .STERADIAN. ) SOLID_ANGLE_UNIT ( ) );
#17775 = AXIS2_PLACEMENT_3D ( 'NONE', #1468, #13930, #10288 ) ;
#17776 = ADVANCED_FACE ( 'NONE', ( #413 ), #15207, .F. ) ;
#17777 = CIRCLE ( 'NONE', #13274, 2.249999999999996003 ) ;
#17778 = ORIENTED_EDGE ( 'NONE', *, *, #1118, .F. ) ;
#17779 = CONICAL_SURFACE ( 'NONE', #10633, 4.750000000000000888, 1.047197551196600074 ) ;
#17780 =( NAMED_UNIT ( * ) SI_UNIT ( $, .STERADIAN. ) SOLID_ANGLE_UNIT ( ) );
#17782 = VERTEX_POINT ( 'NONE', #2401 ) ;
#17781 = ORIENTED_EDGE ( 'NONE', *, *, #8838, .T. ) ;
#17783 = APPLICATION_CONTEXT ( 'automotive_design' ) ;
#17784 = EDGE_CURVE ( 'NONE', #12152, #12647, #7926, .T. ) ;
#17785 = ORIENTED_EDGE ( 'NONE', *, *, #16998, .T. ) ;
#17787 = ORIENTED_EDGE ( 'NONE', *, *, #196, .T. ) ;
#17786 = ORIENTED_EDGE ( 'NONE', *, *, #16304, .T. ) ;
#17788 = ORIENTED_EDGE ( 'NONE', *, *, #19, .T. ) ;
#17789 = DIRECTION ( 'NONE',  ( 3.885780586188016830E-16, 4.437342591868156373E-31, -1.000000000000000000 ) ) ;
#17790 = CARTESIAN_POINT ( 'NONE',  ( -61.45000000000046469, 6.301625887772388776E-14, -1.999999999999973577 ) ) ;
#17791 = CARTESIAN_POINT ( 'NONE',  ( -6.999999999999992006, -12.60977222864646485, 9.250000000000078160 ) ) ;
#17792 = CIRCLE ( 'NONE', #22290, 0.5000000000000022204 ) ;
#17793 = FACE_OUTER_BOUND ( 'NONE', #7062, .T. ) ;
#17794 = VECTOR ( 'NONE', #4099, 1000.000000000000000 ) ;
#17795 = CARTESIAN_POINT ( 'NONE',  ( 22.49999999999998934, 4.250000000000017764, -19.00000000000001421 ) ) ;
#17796 = CIRCLE ( 'NONE', #20816, 4.500000000000052403 ) ;
#17797 = CARTESIAN_POINT ( 'NONE',  ( 0.000000000000000000, 2.775557561562891351E-14, 17.49999999999997513 ) ) ;
#17798 = AXIS2_PLACEMENT_3D ( 'NONE', #16737, #2983, #22279 ) ;
#17799 = DIRECTION ( 'NONE',  ( 0.7071067811865457964, 0.7071067811865492381, 0.000000000000000000 ) ) ;
#17800 = VECTOR ( 'NONE', #601, 1000.000000000000000 ) ;
#17801 = AXIS2_PLACEMENT_3D ( 'NONE', #1335, #10492, #4956 ) ;
#17802 = DIRECTION ( 'NONE',  ( -1.214306433183769502E-15, -6.741645191078037727E-32, 1.000000000000000000 ) ) ;
#17803 = DIRECTION ( 'NONE',  ( -3.885780586188016830E-16, -4.437342591868156373E-31, 1.000000000000000000 ) ) ;
#17804 = PLANE ( 'NONE',  #20448 ) ;
#17805 = LINE ( 'NONE', #19685, #5733 ) ;
#17806 = DIRECTION ( 'NONE',  ( 0.6819983600624981435, -0.7313537016191709039, 0.000000000000000000 ) ) ;
#17807 = LINE ( 'NONE', #10737, #290 ) ;
#17808 = CARTESIAN_POINT ( 'NONE',  ( -4.000000000000476952, -0.8232339106132060547, -3.430630286862590417 ) ) ;
#17809 = CARTESIAN_POINT ( 'NONE',  ( 3.961551342854460867, -3.742715940867668234, 0.5174258321192414245 ) ) ;
#17810 = ORIENTED_EDGE ( 'NONE', *, *, #7212, .F. ) ;
#17811 = VECTOR ( 'NONE', #22783, 1000.000000000000000 ) ;
#17812 =( LENGTH_UNIT ( ) NAMED_UNIT ( * ) SI_UNIT ( .MILLI., .METRE. ) );
#17813 = AXIS2_PLACEMENT_3D ( 'NONE', #18036, #16131, #8979 ) ;
#17814 = B_SPLINE_CURVE_WITH_KNOTS ( 'NONE', 3,
 ( #15689, #5594, #7577, #20166, #18282 ),
 .UNSPECIFIED., .F., .F.,
 ( 4, 1, 4 ),
 ( 0.000000000000000000, 0.002309401076758508826, 0.004618802153517017652 ),
 .UNSPECIFIED. ) ;
#17816 = EDGE_LOOP ( 'NONE', ( #16223, #5336, #7182, #1009 ) ) ;
#17815 = ORIENTED_EDGE ( 'NONE', *, *, #22926, .F. ) ;
#17817 = AXIS2_PLACEMENT_3D ( 'NONE', #17850, #12424, #14206 ) ;
#17818 = ORIENTED_EDGE ( 'NONE', *, *, #6535, .F. ) ;
#17820 = ORIENTED_EDGE ( 'NONE', *, *, #21096, .T. ) ;
#17819 = VERTEX_POINT ( 'NONE', #7815 ) ;
#17821 = ORIENTED_EDGE ( 'NONE', *, *, #22835, .T. ) ;
#17822 = VERTEX_POINT ( 'NONE', #5940 ) ;
#17823 = ORIENTED_EDGE ( 'NONE', *, *, #32, .F. ) ;
#17824 = CARTESIAN_POINT ( 'NONE',  ( -3.499999999708153453, 2.999999999003851503, -26.00000000000000000 ) ) ;
#17825 = CARTESIAN_POINT ( 'NONE',  ( 7.499999999999978684, -1.390227771353540920, 9.250000000000021316 ) ) ;
#17826 = FACE_OUTER_BOUND ( 'NONE', #3660, .T. ) ;
#17827 = DIRECTION ( 'NONE',  ( -2.753132232808505576E-17, 0.6666666666666667407, -0.7453559924999297870 ) ) ;
#17828 = EDGE_CURVE ( 'NONE', #5440, #15768, #4511, .T. ) ;
#17829 = VECTOR ( 'NONE', #5451, 1000.000000000000114 ) ;
#17830 = DIRECTION ( 'NONE',  ( 1.000000000000000000, 1.910522504832140594E-31, -5.551115123125818447E-17 ) ) ;
#17831 = AXIS2_PLACEMENT_3D ( 'NONE', #1657, #5066, #12222 ) ;
#17832 = CARTESIAN_POINT ( 'NONE',  ( 42.00000000000012079, 0.000000000000000000, -12.49999999999999645 ) ) ;
#17833 = CARTESIAN_POINT ( 'NONE',  ( -4.204015924366279577, 1.626724848190933770, -3.610627190413417509 ) ) ;
#17834 = VECTOR ( 'NONE', #16519, 1000.000000000000000 ) ;
#17835 = DIRECTION ( 'NONE',  ( -0.7313537016191749007, 0.6819983600624938136, -2.779290820238839172E-15 ) ) ;
#17836 = DIRECTION ( 'NONE',  ( 2.775557561562824791E-17, 0.000000000000000000, 1.000000000000000000 ) ) ;
#17837 = CARTESIAN_POINT ( 'NONE',  ( 0.000000000000000000, 0.000000000000000000, -4.974599999999998801 ) ) ;
#17838 = DIRECTION ( 'NONE',  ( 1.000000000000000000, -7.477632011778292156E-48, 3.885780586188017323E-16 ) ) ;
#17839 = ORIENTED_EDGE ( 'NONE', *, *, #16974, .T. ) ;
#17840 =( NAMED_UNIT ( * ) SI_UNIT ( $, .STERADIAN. ) SOLID_ANGLE_UNIT ( ) );
#17841 = DIRECTION ( 'NONE',  ( -2.013525853228508439E-32, -6.779273404243028164E-31, 1.000000000000000000 ) ) ;
#17842 = CARTESIAN_POINT ( 'NONE',  ( 1.387778780781445676E-14, 4.618802153517020059, -5.242734410091827613 ) ) ;
#17844 = ORIENTED_EDGE ( 'NONE', *, *, #3475, .F. ) ;
#17843 = VERTEX_POINT ( 'NONE', #4154 ) ;
#17845 = CIRCLE ( 'NONE', #8457, 6.000000000000047073 ) ;
#17846 = ORIENTED_EDGE ( 'NONE', *, *, #17270, .F. ) ;
#17847 = VECTOR ( 'NONE', #1333, 1000.000000000000000 ) ;
#17848 = EDGE_LOOP ( 'NONE', ( #895, #4820, #17221, #6877 ) ) ;
#17849 = ADVANCED_FACE ( 'NONE', ( #6175 ), #2164, .T. ) ;
#17850 = CARTESIAN_POINT ( 'NONE',  ( 124.5000000000017195, -4.000000000000058620, 1.387778780781445676E-14 ) ) ;
#17851 = CARTESIAN_POINT ( 'NONE',  ( 12.84999999999997300, -14.00000000000003020, 5.750000000000032863 ) ) ;
#17852 = CARTESIAN_POINT ( 'NONE',  ( -5.484827557301438894, 1.325747111984031834, 0.000000000000000000 ) ) ;
#17853 = CYLINDRICAL_SURFACE ( 'NONE', #15085, 0.5000000000000036637 ) ;
#17854 = EDGE_CURVE ( 'NONE', #22258, #22523, #21584, .T. ) ;
#17855 = CARTESIAN_POINT ( 'NONE',  ( -6.938893903907228378E-15, -12.15667283655309028, 0.000000000000000000 ) ) ;
#17856 = DIRECTION ( 'NONE',  ( -1.000000000000000000, -4.440892098500626162E-16, 5.551115123125782702E-16 ) ) ;
#17857 = DIRECTION ( 'NONE',  ( 0.000000000000000000, 0.000000000000000000, 1.000000000000000000 ) ) ;
#17858 = CARTESIAN_POINT ( 'NONE',  ( 4.113620667976075396, 1.750000000000001554, -2.375000000000002220 ) ) ;
#17859 = FACE_OUTER_BOUND ( 'NONE', #2530, .T. ) ;
#17860 = AXIS2_PLACEMENT_3D ( 'NONE', #22571, #10103, #15501 ) ;
#17861 = EDGE_CURVE ( 'NONE', #16898, #10216, #11226, .T. ) ;
#17862 = VECTOR ( 'NONE', #4576, 1000.000000000000000 ) ;
#17863 = EDGE_CURVE ( 'NONE', #19813, #14653, #16505, .T. ) ;
#17864 = DIRECTION ( 'NONE',  ( 1.000000000000000000, -4.437342591868175641E-31, 3.330669073875457788E-16 ) ) ;
#17865 = CARTESIAN_POINT ( 'NONE',  ( 2.119223235054759529E-14, 10.00000000000000533, 2.500000000000006661 ) ) ;
#17867 = EDGE_CURVE ( 'NONE', #18765, #5339, #2406, .T. ) ;
#17866 = CARTESIAN_POINT ( 'NONE',  ( 37.00000000000011369, 11.00000000000000000, -10.00000000000000888 ) ) ;
#17868 = CARTESIAN_POINT ( 'NONE',  ( 109.2950040998454710, -11.69922134891568355, 6.000000000000067502 ) ) ;
#17869 = LINE ( 'NONE', #16082, #14931 ) ;
#17870 = EDGE_LOOP ( 'NONE', ( #12092, #10467 ) ) ;
#17871 = EDGE_LOOP ( 'NONE', ( #373, #6524 ) ) ;
#17872 = EDGE_CURVE ( 'NONE', #14621, #10396, #21215, .T. ) ;
#17873 = CARTESIAN_POINT ( 'NONE',  ( -6.977878452269129284, 35.99999999900352776, -26.49046115436484783 ) ) ;
#17874 = ADVANCED_FACE ( 'NONE', ( #4044 ), #13679, .T. ) ;
#17875 = EDGE_LOOP ( 'NONE', ( #21266, #421, #23205, #19314 ) ) ;
#17876 = DIRECTION ( 'NONE',  ( -1.000000000000000000, -2.699383410053119644E-30, -3.330669073875432643E-16 ) ) ;
#17877 = CARTESIAN_POINT ( 'NONE',  ( 6.500000000000005329, 0.5000000000001669775, 3.469446951953614189E-14 ) ) ;
#17878 = DIRECTION ( 'NONE',  ( -1.000000000000000000, -1.479114197289397135E-31, 7.395570986446975166E-31 ) ) ;
#17879 = ORIENTED_EDGE ( 'NONE', *, *, #3494, .F. ) ;
#17880 = CIRCLE ( 'NONE', #12612, 7.000000000000075495 ) ;
#17881 = DIRECTION ( 'NONE',  ( -7.860214984770699307E-18, 1.409037165336591006E-16, 1.000000000000000000 ) ) ;
#17882 = LINE ( 'NONE', #8943, #13435 ) ;
#17883 = ADVANCED_FACE ( 'NONE', ( #20525 ), #7433, .F. ) ;
#17884 = DIRECTION ( 'NONE',  ( 1.000000000000000000, 1.479114197289397573E-31, 0.000000000000000000 ) ) ;
#17885 = DIRECTION ( 'NONE',  ( 1.000000000000000000, -1.424116703980815236E-16, -2.931272055834072201E-32 ) ) ;
#17886 = CIRCLE ( 'NONE', #14134, 6.000000000000047073 ) ;
#17887 = CARTESIAN_POINT ( 'NONE',  ( 37.00000000000014211, 10.75000000000000000, -2.566987298107808790 ) ) ;
#17888 = FACE_OUTER_BOUND ( 'NONE', #19340, .T. ) ;
#17889 = EDGE_CURVE ( 'NONE', #17191, #15879, #4623, .T. ) ;
#17890 = DIRECTION ( 'NONE',  ( -1.756300210255732376E-61, 4.190823558986625216E-31, 1.000000000000000000 ) ) ;
#17891 = CARTESIAN_POINT ( 'NONE',  ( 4.055492966679551614, -3.795017426214470913, 0.5629142681440486573 ) ) ;
#17893 = EDGE_CURVE ( 'NONE', #2089, #15881, #5052, .T. ) ;
#17892 = CARTESIAN_POINT ( 'NONE',  ( -4.113620667976075396, 1.749999999999998002, 2.374999999999998668 ) ) ;
#17894 = CARTESIAN_POINT ( 'NONE',  ( 8.660254037844337560, 4.999999999999948486, 2.775557561562891351E-14 ) ) ;
#17895 = AXIS2_PLACEMENT_3D ( 'NONE', #21968, #16311, #11015 ) ;
#17896 = ORIENTED_EDGE ( 'NONE', *, *, #15692, .T. ) ;
#17897 = VECTOR ( 'NONE', #20335, 1000.000000000000000 ) ;
#17898 = DIRECTION ( 'NONE',  ( -6.479283114852342540E-12, -9.090171498299720443E-12, 1.000000000000000000 ) ) ;
#17899 = B_SPLINE_CURVE_WITH_KNOTS ( 'NONE', 3,
 ( #8439, #11601, #19130, #15476 ),
 .UNSPECIFIED., .F., .F.,
 ( 4, 4 ),
 ( 0.000000000000000000, 0.002080789711329285828 ),
 .UNSPECIFIED. ) ;
#17901 = VERTEX_POINT ( 'NONE', #17316 ) ;
#17900 = EDGE_LOOP ( 'NONE', ( #6731, #17903 ) ) ;
#17902 = AXIS2_PLACEMENT_3D ( 'NONE', #8893, #12410, #10423 ) ;
#17903 = ORIENTED_EDGE ( 'NONE', *, *, #13983, .T. ) ;
#17905 = ORIENTED_EDGE ( 'NONE', *, *, #5357, .F. ) ;
#17904 = ORIENTED_EDGE ( 'NONE', *, *, #10404, .F. ) ;
#17906 = CARTESIAN_POINT ( 'NONE',  ( 0.000000000000000000, 0.000000000000000000, -4.000000000000000000 ) ) ;
#17907 = DIRECTION ( 'NONE',  ( 3.512600420511457844E-61, -4.190823558986624340E-31, -1.000000000000000000 ) ) ;
#17908 = CARTESIAN_POINT ( 'NONE',  ( 7.638377885296781855, -12.06377841978598831, 8.340398698103349773 ) ) ;
#17909 = CARTESIAN_POINT ( 'NONE',  ( -8.438463404362684273, -11.99816466695113526, 6.398712851742201835 ) ) ;
#17910 = EDGE_CURVE ( 'NONE', #5689, #9100, #6548, .T. ) ;
#17911 = CARTESIAN_POINT ( 'NONE',  ( 63.53596085922837489, -2.925414806476733798, -6.499999999999957367 ) ) ;
#17912 = CARTESIAN_POINT ( 'NONE',  ( 7.733764002503177970, -13.25269934883866441, 8.082002268151514457 ) ) ;
#17913 = CARTESIAN_POINT ( 'NONE',  ( -64.00000000000045475, -7.632783294297951215E-14, -2.000000000000001776 ) ) ;
#17914 = DIRECTION ( 'NONE',  ( 1.000000000000000000, -1.276756478318922922E-15, 1.288690253661653294E-15 ) ) ;
#17915 = CIRCLE ( 'NONE', #19794, 3.999999999999999112 ) ;
#17916 = CARTESIAN_POINT ( 'NONE',  ( 4.113620667976075396, 1.750000000000001554, -2.375000000000002220 ) ) ;
#17917 = CARTESIAN_POINT ( 'NONE',  ( 81.85734743794770907, -6.246200939475199831, 6.000000000000102141 ) ) ;
#17918 = CYLINDRICAL_SURFACE ( 'NONE', #23013, 0.4999999999999995559 ) ;
#17919 = EDGE_CURVE ( 'NONE', #16028, #10146, #19208, .T. ) ;
#17920 = CIRCLE ( 'NONE', #13767, 5.000000000000000888 ) ;
#17921 = FACE_OUTER_BOUND ( 'NONE', #16920, .T. ) ;
#17922 = CARTESIAN_POINT ( 'NONE',  ( 7.026577802269673434, -2.648906230146660601, 8.453373545151620760 ) ) ;
#17923 = CARTESIAN_POINT ( 'NONE',  ( -4.000000000000107470, -1.680117682357857412, -3.316611593219131571 ) ) ;
#17924 = CARTESIAN_POINT ( 'NONE',  ( 7.525553787417718965, -1.070926652787001609, 8.786654903594095956 ) ) ;
#17925 = ORIENTED_EDGE ( 'NONE', *, *, #8112, .F. ) ;
#17926 = SHAPE_REPRESENTATION_RELATIONSHIP ( 'NONE' , 'NONE' ,  #17033, #3025 ) ;
#17928 = EDGE_LOOP ( 'NONE', ( #21327, #13587, #10744, #19083 ) ) ;
#17927 = ORIENTED_EDGE ( 'NONE', *, *, #13524, .T. ) ;
#17929 = EDGE_LOOP ( 'NONE', ( #11844, #12890, #19194, #20689 ) ) ;
#17931 = EDGE_LOOP ( 'NONE', ( #17245, #9021, #13902, #5750 ) ) ;
#17930 = ORIENTED_EDGE ( 'NONE', *, *, #11252, .T. ) ;
#17932 = EDGE_LOOP ( 'NONE', ( #17879, #146, #7661, #8470, #9136, #9223, #1267, #9331, #12654, #11606, #8609, #1811, #22152 ) ) ;
#17933 = CIRCLE ( 'NONE', #17531, 4.749999999999986677 ) ;
#17934 = ORIENTED_EDGE ( 'NONE', *, *, #11241, .T. ) ;
#17935 = ORIENTED_EDGE ( 'NONE', *, *, #18576, .F. ) ;
#17936 = PLANE ( 'NONE',  #20474 ) ;
#17937 = CIRCLE ( 'NONE', #13044, 2.500000000000015987 ) ;
#17938 = FILL_AREA_STYLE_COLOUR ( '', #500 ) ;
#17939 = EDGE_CURVE ( 'NONE', #20683, #12123, #11411, .T. ) ;
#17940 = PLANE ( 'NONE',  #16512 ) ;
#17941 = FACE_OUTER_BOUND ( 'NONE', #15573, .T. ) ;
#17942 = AXIS2_PLACEMENT_3D ( 'NONE', #11680, #16315, #15210 ) ;
#17943 = DIRECTION ( 'NONE',  ( 1.000000000000000000, 0.000000000000000000, 0.000000000000000000 ) ) ;
#17944 = CARTESIAN_POINT ( 'NONE',  ( 22.49999999999992539, 1.999999999999960032, -18.75000000000001421 ) ) ;
#17945 = CARTESIAN_POINT ( 'NONE',  ( -4.198928548860862087, 0.8158838809860016195, -3.526471437616944815 ) ) ;
#17946 = SURFACE_STYLE_FILL_AREA ( #19824 ) ;
#17947 = CIRCLE ( 'NONE', #20585, 2.000000000000015543 ) ;
#17948 = EDGE_CURVE ( 'NONE', #14077, #15916, #16302, .T. ) ;
#17949 = DIRECTION ( 'NONE',  ( 0.000000000000000000, 0.000000000000000000, 1.000000000000000000 ) ) ;
#17950 = CARTESIAN_POINT ( 'NONE',  ( 5.213674118230995802, 0.7500000000000561773, -1.500000000000001332 ) ) ;
#17951 =( BOUNDED_SURFACE ( )  B_SPLINE_SURFACE ( 3, 2, ( 
 ( #15749, #8584, #16201 ),
 ( #10806, #3412, #15854 ),
 ( #1643, #5053, #17999 ),
 ( #14231, #116, #21421 ),
 ( #14463, #10573, #21647 ),
 ( #8822, #15974, #1408 ) ),
 .UNSPECIFIED., .F., .F., .T. ) 
 B_SPLINE_SURFACE_WITH_KNOTS ( ( 4, 2, 4 ),
 ( 3, 3 ),
 ( 0.02032853247518128306, 0.02278863295364823988, 0.02524873343211519669 ),
 ( 0.000000000000000000, 1.000000000000000000 ),
 .UNSPECIFIED. ) 
 GEOMETRIC_REPRESENTATION_ITEM ( )  RATIONAL_B_SPLINE_SURFACE ( (
 ( 1.000000000000000000, 0.8047781615896822949, 1.000000000000000000),
 ( 1.000000000000000000, 0.8123767586288903608, 1.000000000000000000),
 ( 1.000000000000000000, 0.8190662415564858856, 1.000000000000000000),
 ( 1.000000000000000000, 0.8192361015668548907, 1.000000000000000000),
 ( 1.000000000000000000, 0.8126135807104273301, 1.000000000000000000),
 ( 1.000000000000000000, 0.8047712338318591119, 1.000000000000000000) ) ) 
 REPRESENTATION_ITEM ( '' )  SURFACE ( )  );
#17952 = CARTESIAN_POINT ( 'NONE',  ( -4.920724633012840243, 13.68667664578917709, -16.13822288903187996 ) ) ;
#17953 = VECTOR ( 'NONE', #8104, 1000.000000000000114 ) ;
#17954 = FACE_OUTER_BOUND ( 'NONE', #14769, .T. ) ;
#17955 = CIRCLE ( 'NONE', #7420, 0.4999999999999995559 ) ;
#17956 = ORIENTED_EDGE ( 'NONE', *, *, #16245, .F. ) ;
#17957 = DIRECTION ( 'NONE',  ( 0.000000000000000000, 0.000000000000000000, 1.000000000000000000 ) ) ;
#17958 = LINE ( 'NONE', #5372, #7859 ) ;
#17959 = DIRECTION ( 'NONE',  ( 3.254448077146059901E-32, 1.000000000000000000, -6.656013887802287108E-31 ) ) ;
#17961 = ORIENTED_EDGE ( 'NONE', *, *, #19019, .F. ) ;
#17960 = ORIENTED_EDGE ( 'NONE', *, *, #3507, .F. ) ;
#17962 = CIRCLE ( 'NONE', #18321, 4.000000000000023981 ) ;
#17963 = ADVANCED_FACE ( 'NONE', ( #3226 ), #4741, .F. ) ;
#17964 = COLOUR_RGB ( '', 0.08235294, 0.09019608, 0.10196078) ;
#17965 = ORIENTED_EDGE ( 'NONE', *, *, #14260, .T. ) ;
#17966 = ORIENTED_EDGE ( 'NONE', *, *, #18691, .T. ) ;
#17967 = ORIENTED_EDGE ( 'NONE', *, *, #5831, .F. ) ;
#17968 = DIRECTION ( 'NONE',  ( 3.885780586187959638E-16, 0.000000000000000000, -1.000000000000000000 ) ) ;
#17969 = CARTESIAN_POINT ( 'NONE',  ( 7.644579933246795633, -0.8425218428686449545, 8.321099285265821877 ) ) ;
#17970 = DIRECTION ( 'NONE',  ( -2.013525853228507892E-32, -6.902532920683810383E-31, 1.000000000000000000 ) ) ;
#17971 = VECTOR ( 'NONE', #15939, 1000.000000000000000 ) ;
#17972 = CARTESIAN_POINT ( 'NONE',  ( 37.18301270189238039, 0.09150635094611105080, -10.52451905283837519 ) ) ;
#17973 = DIRECTION ( 'NONE',  ( 2.172745813409349776E-17, -1.000000000000000000, 1.309377075419428048E-16 ) ) ;
#17974 = DIRECTION ( 'NONE',  ( 0.000000000000000000, -1.000000000000000000, 0.000000000000000000 ) ) ;
#17975 = AXIS2_PLACEMENT_3D ( 'NONE', #7042, #19848, #9144 ) ;
#17976 = CARTESIAN_POINT ( 'NONE',  ( 7.955953741309954808, -12.35582749618195741, 7.654083333123934629 ) ) ;
#17977 = CARTESIAN_POINT ( 'NONE',  ( -3.200000000000049916, 5.299999999999957190, -7.500000000000034639 ) ) ;
#17978 = CARTESIAN_POINT ( 'NONE',  ( 10.49999999999998224, -0.5000000000000004441, 6.250000000000061284 ) ) ;
#17979 = AXIS2_PLACEMENT_3D ( 'NONE', #3074, #8486, #15645 ) ;
#17980 = CARTESIAN_POINT ( 'NONE',  ( 37.45482484129324519, 10.78777973366406329, -10.04362427881554964 ) ) ;
#17981 = VECTOR ( 'NONE', #3313, 1000.000000000000000 ) ;
#17982 = AXIS2_PLACEMENT_3D ( 'NONE', #13829, #11829, #19232 ) ;
#17983 = LINE ( 'NONE', #1848, #10646 ) ;
#17984 = LINE ( 'NONE', #21637, #17163 ) ;
#17985 = CARTESIAN_POINT ( 'NONE',  ( 5.551115123125782702E-14, 0.2500000000000002220, -2.566987298107781257 ) ) ;
#17986 = PRODUCT_RELATED_PRODUCT_CATEGORY ( 'part', '', ( #18870 ) ) ;
#17987 = CARTESIAN_POINT ( 'NONE',  ( 2.499999999999984901, 2.000000000000001776, -1.500000000000029088 ) ) ;
#17988 = FACE_OUTER_BOUND ( 'NONE', #20387, .T. ) ;
#17989 = ORIENTED_EDGE ( 'NONE', *, *, #20748, .F. ) ;
#17990 = EDGE_CURVE ( 'NONE', #4065, #9788, #18559, .T. ) ;
#17991 = ORIENTED_EDGE ( 'NONE', *, *, #17247, .T. ) ;
#17992 = SHAPE_REPRESENTATION ( 'Lock nut', ( #22115 ), #12003 ) ;
#17993 = CARTESIAN_POINT ( 'NONE',  ( -5.498446330623528056, 36.40058408549441538, -28.60140285650649972 ) ) ;
#17994 = CIRCLE ( 'NONE', #5974, 2.055000000000002380 ) ;
#17996 = ADVANCED_FACE ( 'NONE', ( #11909 ), #10765, .F. ) ;
#17995 = VERTEX_POINT ( 'NONE', #10268 ) ;
#17997 = VECTOR ( 'NONE', #10875, 1000.000000000000114 ) ;
#17998 = CIRCLE ( 'NONE', #18722, 0.5000000000000002220 ) ;
#17999 = CARTESIAN_POINT ( 'NONE',  ( 1.360585162434879036, -4.061296242128364042, -3.505054077164883264 ) ) ;
#18000 = EDGE_CURVE ( 'NONE', #7880, #2970, #15546, .T. ) ;
#18001 = DIRECTION ( 'NONE',  ( 0.000000000000000000, 0.000000000000000000, 1.000000000000000000 ) ) ;
#18002 = EDGE_LOOP ( 'NONE', ( #19339, #725, #19605, #10246, #14480 ) ) ;
#18003 = LINE ( 'NONE', #23187, #9900 ) ;
#18004 = CARTESIAN_POINT ( 'NONE',  ( 0.2265654810057098067, 0.6000000000000128564, -3.877828006771827596 ) ) ;
#18005 = DIRECTION ( 'NONE',  ( -4.190823558986625216E-31, 1.000000000000000000, -4.190823558986625216E-31 ) ) ;
#18006 = FACE_OUTER_BOUND ( 'NONE', #10284, .T. ) ;
#18007 =( GEOMETRIC_REPRESENTATION_CONTEXT ( 3 ) GLOBAL_UNCERTAINTY_ASSIGNED_CONTEXT ( ( #4839 ) ) GLOBAL_UNIT_ASSIGNED_CONTEXT ( ( #16167, #85, #17840 ) ) REPRESENTATION_CONTEXT ( 'NONE', 'WORKASPACE' ) );
#18008 = CARTESIAN_POINT ( 'NONE',  ( 37.86602540378461157, 11.00000000000000000, -2.133974596215532316 ) ) ;
#18009 = CARTESIAN_POINT ( 'NONE',  ( 3.999999999999952482, -1.539600717839022082, -3.300726591567082036 ) ) ;
#18010 = DIRECTION ( 'NONE',  ( -0.9706398123736330597, 1.505375731439247434E-16, -0.2405376366294442736 ) ) ;
#18011 = CARTESIAN_POINT ( 'NONE',  ( 4.158806965674314071, -4.075748668184007606, -0.05940377217584739272 ) ) ;
#18012 = CARTESIAN_POINT ( 'NONE',  ( -2.966164998648741058, 1.454929939081821999, 4.362451518707897158 ) ) ;
#18013 = EDGE_CURVE ( 'NONE', #6303, #7694, #16533, .T. ) ;
#18014 = VECTOR ( 'NONE', #11713, 1000.000000000000000 ) ;
#18015 = EDGE_CURVE ( 'NONE', #3763, #7940, #16242, .T. ) ;
#18016 = DIRECTION ( 'NONE',  ( 1.000000000000000000, 4.356083395230605100E-14, 3.854941057726199147E-16 ) ) ;
#18017 = EDGE_LOOP ( 'NONE', ( #13977, #10278, #6062 ) ) ;
#18018 = EDGE_CURVE ( 'NONE', #13552, #5016, #21949, .T. ) ;
#18019 = APPLICATION_PROTOCOL_DEFINITION ( 'draft international standard', 'automotive_design', 1998, #19916 ) ;
#18020 = STYLED_ITEM ( 'NONE', ( #3746 ), #13352 ) ;
#18022 = ORIENTED_EDGE ( 'NONE', *, *, #9374, .F. ) ;
#18021 = VERTEX_POINT ( 'NONE', #19915 ) ;
#18025 = VERTEX_POINT ( 'NONE', #14271 ) ;
#18024 = EDGE_CURVE ( 'NONE', #2907, #21787, #14062, .T. ) ;
#18023 = ORIENTED_EDGE ( 'NONE', *, *, #13997, .F. ) ;
#18026 = EDGE_CURVE ( 'NONE', #17226, #2694, #19437, .T. ) ;
#18027 = CARTESIAN_POINT ( 'NONE',  ( 0.000000000000000000, 0.000000000000000000, -4.694516984716116781 ) ) ;
#18028 = FACE_OUTER_BOUND ( 'NONE', #18419, .T. ) ;
#18029 = CARTESIAN_POINT ( 'NONE',  ( -7.761744141695584354, -11.93564195219169477, 6.973942750959578163 ) ) ;
#18030 = DIRECTION ( 'NONE',  ( 1.134196829589822059E-15, 6.741645191078038822E-32, -1.000000000000000000 ) ) ;
#18031 = CARTESIAN_POINT ( 'NONE',  ( 124.5000000000018332, -7.000000000000006217, 6.000000000000088818 ) ) ;
#18032 = CARTESIAN_POINT ( 'NONE',  ( 0.000000000000000000, 0.000000000000000000, 0.000000000000000000 ) ) ;
#18033 = DIRECTION ( 'NONE',  ( 2.220446049250313081E-16, -1.000000000000000000, 7.025792437124636392E-31 ) ) ;
#18034 = CARTESIAN_POINT ( 'NONE',  ( 3.649122391096871532, 1.701165921963294858, -3.179534615583005763 ) ) ;
#18035 = CIRCLE ( 'NONE', #26, 0.5000000000000000000 ) ;
#18036 = CARTESIAN_POINT ( 'NONE',  ( -12.84999999999999964, -2.000000000000001776, 0.000000000000000000 ) ) ;
#18037 = EDGE_CURVE ( 'NONE', #13010, #3689, #263, .T. ) ;
#18038 = CARTESIAN_POINT ( 'NONE',  ( 4.578118944855307682, -1.701165921963294858, -1.570465384417001786 ) ) ;
#18039 = ADVANCED_FACE ( 'NONE', ( #14377 ), #5564, .F. ) ;
#18040 = AXIS2_PLACEMENT_3D ( 'NONE', #15420, #22605, #6494 ) ;
#18041 = FACE_OUTER_BOUND ( 'NONE', #21140, .T. ) ;
#18042 = ADVANCED_FACE ( 'NONE', ( #5327 ), #2029, .T. ) ;
#18043 = DIRECTION ( 'NONE',  ( 1.000000000000000000, 2.699383410053119644E-30, 3.330669073875432643E-16 ) ) ;
#18044 = CARTESIAN_POINT ( 'NONE',  ( 2.918498775983380256E-10, -9.961476088449217059E-10, 0.000000000000000000 ) ) ;
#18045 = CARTESIAN_POINT ( 'NONE',  ( 7.490952241692643732, -0.6544882962155422756, 8.992386117842515958 ) ) ;
#18046 = EDGE_LOOP ( 'NONE', ( #540, #5531, #14537, #20040 ) ) ;
#18048 = ORIENTED_EDGE ( 'NONE', *, *, #8096, .T. ) ;
#18047 = ORIENTED_EDGE ( 'NONE', *, *, #14703, .F. ) ;
#18049 = UNCERTAINTY_MEASURE_WITH_UNIT (LENGTH_MEASURE( 1.000000000000000082E-05 ), #441, 'distance_accuracy_value', 'NONE');
#18050 = EDGE_CURVE ( 'NONE', #21787, #8580, #19796, .T. ) ;
#18051 = EDGE_LOOP ( 'NONE', ( #7592, #10741, #17330, #21473, #1248 ) ) ;
#18054 = ORIENTED_EDGE ( 'NONE', *, *, #6951, .F. ) ;
#18053 = ORIENTED_EDGE ( 'NONE', *, *, #21203, .F. ) ;
#18052 = EDGE_CURVE ( 'NONE', #9560, #15339, #18146, .T. ) ;
#18055 = CIRCLE ( 'NONE', #15023, 2.000000000000015543 ) ;
#18056 = ORIENTED_EDGE ( 'NONE', *, *, #19611, .F. ) ;
#18057 = DIRECTION ( 'NONE',  ( 0.8660254037844379305, 0.5000000000000012212, 1.169077423688995342E-15 ) ) ;
#18058 = ORIENTED_EDGE ( 'NONE', *, *, #4501, .F. ) ;
#18059 = ORIENTED_EDGE ( 'NONE', *, *, #18823, .T. ) ;
#18060 = CARTESIAN_POINT ( 'NONE',  ( -10.49999999999998224, -12.50000000000002842, 6.250000000000061284 ) ) ;
#18061 = CARTESIAN_POINT ( 'NONE',  ( -95.20000000000061391, -9.714451465470119729E-14, 1.000000000000028644 ) ) ;
#18062 = CARTESIAN_POINT ( 'NONE',  ( -6.938893903907228378E-15, -12.15667283655309028, 0.000000000000000000 ) ) ;
#18063 = CARTESIAN_POINT ( 'NONE',  ( 12.49999999999992362, 1.500000000000015099, -4.500000000000003553 ) ) ;
#18064 = LINE ( 'NONE', #13109, #14767 ) ;
#18065 = CYLINDRICAL_SURFACE ( 'NONE', #10847, 0.5000000000000012212 ) ;
#18066 = CARTESIAN_POINT ( 'NONE',  ( -2.742827927723580306, -3.035229711104924899, -3.433252694550618767 ) ) ;
#18067 =( NAMED_UNIT ( * ) SI_UNIT ( $, .STERADIAN. ) SOLID_ANGLE_UNIT ( ) );
#18068 = DIRECTION ( 'NONE',  ( 1.000000000000000000, 4.440892098500626162E-16, -5.551115123125782702E-16 ) ) ;
#18069 = AXIS2_PLACEMENT_3D ( 'NONE', #1081, #13657, #9773 ) ;
#18070 = DIRECTION ( 'NONE',  ( 3.885780586188016830E-16, 4.437342591868156373E-31, -1.000000000000000000 ) ) ;
#18071 = CARTESIAN_POINT ( 'NONE',  ( 37.69139372032810797, 10.99999999999995914, -2.221290437944332119 ) ) ;
#18072 = EDGE_LOOP ( 'NONE', ( #13788, #10542, #19691, #20447 ) ) ;
#18073 = CARTESIAN_POINT ( 'NONE',  ( -10.49999999999999467, -13.50000000000000888, 9.250000000000035527 ) ) ;
#18075 = VERTEX_POINT ( 'NONE', #12731 ) ;
#18074 = ORIENTED_EDGE ( 'NONE', *, *, #22180, .F. ) ;
#18076 = VERTEX_POINT ( 'NONE', #14613 ) ;
#18077 = EDGE_LOOP ( 'NONE', ( #10748, #16001, #19392, #10965 ) ) ;
#18078 = ORIENTED_EDGE ( 'NONE', *, *, #4211, .F. ) ;
#18079 = EDGE_CURVE ( 'NONE', #19457, #3351, #12917, .T. ) ;
#18080 = CARTESIAN_POINT ( 'NONE',  ( 83.98338480886823731, -11.64708151429766403, 6.500000000000117240 ) ) ;
#18081 = CIRCLE ( 'NONE', #3793, 0.5000000000000004441 ) ;
#18082 = DIRECTION ( 'NONE',  ( -1.387778780781445676E-14, -1.000000000000000000, 0.000000000000000000 ) ) ;
#18083 = LINE ( 'NONE', #1948, #20180 ) ;
#18084 = CARTESIAN_POINT ( 'NONE',  ( -1.110223024625156540E-13, -1.999999999999988010, 7.500000000000020428 ) ) ;
#18085 = FACE_OUTER_BOUND ( 'NONE', #8605, .T. ) ;
#18086 = DIRECTION ( 'NONE',  ( 0.000000000000000000, 0.000000000000000000, 1.000000000000000000 ) ) ;
#18087 = CARTESIAN_POINT ( 'NONE',  ( -55.05572809000126711, 1.387778780781445676E-14, -7.500000000000034639 ) ) ;
#18088 = DIRECTION ( 'NONE',  ( 5.551115123125797493E-17, -2.869019762633797485E-16, -1.000000000000000000 ) ) ;
#18089 = LINE ( 'NONE', #2078, #430 ) ;
#18090 = DIRECTION ( 'NONE',  ( 1.000000000000000000, 0.000000000000000000, 0.000000000000000000 ) ) ;
#18091 = FACE_OUTER_BOUND ( 'NONE', #306, .T. ) ;
#18092 = CARTESIAN_POINT ( 'NONE',  ( 77.42435809754134368, -10.99999999999981526, -6.000000000000047073 ) ) ;
#18093 = CARTESIAN_POINT ( 'NONE',  ( -4.692963726980019956, 1.672424706883815393, -1.371548386792625696 ) ) ;
#18094 = PLANE ( 'NONE',  #9342 ) ;
#18095 = DIRECTION ( 'NONE',  ( -0.5000000000000001110, -1.577721810442023611E-30, 0.8660254037844385966 ) ) ;
#18096 = TOROIDAL_SURFACE ( 'NONE', #21105, 2.500000000000003997, 0.5000000000000000000 ) ;
#18097 = ORIENTED_EDGE ( 'NONE', *, *, #4081, .F. ) ;
#18098 = EDGE_LOOP ( 'NONE', ( #15849, #7857, #8789, #12538 ) ) ;
#18099 = LINE ( 'NONE', #18332, #10243 ) ;
#18100 = DIRECTION ( 'NONE',  ( -1.000000000000000000, 0.000000000000000000, -1.066788928082016908E-26 ) ) ;
#18101 = EDGE_LOOP ( 'NONE', ( #18797, #9393, #9499, #7001 ) ) ;
#18102 = CARTESIAN_POINT ( 'NONE',  ( -6.549842551561727788, 36.00336057837472481, -18.61861813964035761 ) ) ;
#18103 = CARTESIAN_POINT ( 'NONE',  ( 3.355112389629148151, -2.681727112203222241, -0.2256878752776871611 ) ) ;
#18104 = CARTESIAN_POINT ( 'NONE',  ( 4.050823680195225762, 3.779313952391327280, -0.5899027668435032901 ) ) ;
#18105 = PLANE ( 'NONE',  #22531 ) ;
#18106 = EDGE_LOOP ( 'NONE', ( #16597, #21113 ) ) ;
#18107 = AXIS2_PLACEMENT_3D ( 'NONE', #3012, #22661, #10179 ) ;
#18108 = AXIS2_PLACEMENT_3D ( 'NONE', #19736, #21510, #5619 ) ;
#18109 = DIRECTION ( 'NONE',  ( 3.032184104443272185E-30, 1.000000000000000000, -7.395570986447005381E-32 ) ) ;
#18110 = CARTESIAN_POINT ( 'NONE',  ( -3.499999999708153453, 38.99999999900385461, -19.00000000000000355 ) ) ;
#18111 = CARTESIAN_POINT ( 'NONE',  ( 7.835312244870012321, -13.94896639302768371, 7.041165740960589225 ) ) ;
#18112 = EDGE_CURVE ( 'NONE', #6039, #21059, #2777, .T. ) ;
#18113 = CARTESIAN_POINT ( 'NONE',  ( -2.081668171172168513E-14, 1.250000000000001110, -2.000000000000001776 ) ) ;
#18114 = DIRECTION ( 'NONE',  ( -1.733449886265890494E-32, 7.264582621685753859E-63, 1.000000000000000000 ) ) ;
#18115 = DIRECTION ( 'NONE',  ( -0.7071067811865449082, 0.7071067811865501263, 0.000000000000000000 ) ) ;
#18116 = CARTESIAN_POINT ( 'NONE',  ( -95.20000000000065654, 0.5000000000000073275, 8.000000000000076383 ) ) ;
#18117 = DIRECTION ( 'NONE',  ( 1.000000000000000000, 1.734723475976796001E-16, 0.000000000000000000 ) ) ;
#18118 = AXIS2_PLACEMENT_3D ( 'NONE', #20986, #22517, #14037 ) ;
#18119 = CARTESIAN_POINT ( 'NONE',  ( 3.999999999999955147, -3.469446951953614189E-14, 0.000000000000000000 ) ) ;
#18120 = ORIENTED_EDGE ( 'NONE', *, *, #12674, .T. ) ;
#18121 = APPLICATION_PROTOCOL_DEFINITION ( 'draft international standard', 'automotive_design', 1998, #14753 ) ;
#18122 = AXIS2_PLACEMENT_3D ( 'NONE', #4377, #16959, #13107 ) ;
#18124 = ORIENTED_EDGE ( 'NONE', *, *, #21755, .T. ) ;
#18123 = VERTEX_POINT ( 'NONE', #47 ) ;
#18125 = AXIS2_PLACEMENT_3D ( 'NONE', #4790, #20691, #16900 ) ;
#18126 = VECTOR ( 'NONE', #669, 1000.000000000000000 ) ;
#18127 = ORIENTED_EDGE ( 'NONE', *, *, #7501, .T. ) ;
#18128 = VECTOR ( 'NONE', #9623, 1000.000000000000000 ) ;
#18130 = VERTEX_POINT ( 'NONE', #16017 ) ;
#18129 = ORIENTED_EDGE ( 'NONE', *, *, #6067, .F. ) ;
#18131 = DIRECTION ( 'NONE',  ( -9.693457064947022734E-26, 0.000000000000000000, 1.000000000000000000 ) ) ;
#18132 = CARTESIAN_POINT ( 'NONE',  ( 37.48161866288226207, 0.1772999597157617346, -2.902788078020140272 ) ) ;
#18133 = EDGE_CURVE ( 'NONE', #17574, #17239, #7308, .T. ) ;
#18134 = LINE ( 'NONE', #12833, #19279 ) ;
#18135 = AXIS2_PLACEMENT_3D ( 'NONE', #21459, #19559, #8861 ) ;
#18136 = DIRECTION ( 'NONE',  ( 0.000000000000000000, 1.000000000000000000, 0.000000000000000000 ) ) ;
#18137 = FACE_OUTER_BOUND ( 'NONE', #22300, .T. ) ;
#18138 = DIRECTION ( 'NONE',  ( -1.454462294001240516E-30, -1.000000000000000000, -0.000000000000000000 ) ) ;
#18139 = ADVANCED_FACE ( 'NONE', ( #9082 ), #21684, .T. ) ;
#18140 = DIRECTION ( 'NONE',  ( -3.070652698126927723E-17, -1.000000000000000000, 4.167305704548413124E-17 ) ) ;
#18141 = DIRECTION ( 'NONE',  ( 0.000000000000000000, 0.000000000000000000, 1.000000000000000000 ) ) ;
#18142 = DIRECTION ( 'NONE',  ( -1.550910762415566494E-16, -1.000000000000000000, 8.135128085091684243E-31 ) ) ;
#18143 = B_SPLINE_CURVE_WITH_KNOTS ( 'NONE', 3,
 ( #6655, #19234, #1372, #13940, #17587, #17470 ),
 .UNSPECIFIED., .F., .F.,
 ( 4, 2, 4 ),
 ( 0.004766700742568914795, 0.006150321122490677583, 0.007533941502412439505 ),
 .UNSPECIFIED. ) ;
#18144 = CARTESIAN_POINT ( 'NONE',  ( 42.00000000000020606, 8.000000000000003553, -15.50000000000004086 ) ) ;
#18145 = CIRCLE ( 'NONE', #8016, 6.000000000000063061 ) ;
#18146 = LINE ( 'NONE', #3781, #4274 ) ;
#18147 = AXIS2_PLACEMENT_3D ( 'NONE', #4870, #12040, #1362 ) ;
#18148 = DIRECTION ( 'NONE',  ( 1.066788928082016908E-26, 3.471809175856251779E-58, -1.000000000000000000 ) ) ;
#18149 = CIRCLE ( 'NONE', #5378, 0.5000000000000017764 ) ;
#18150 = CARTESIAN_POINT ( 'NONE',  ( 4.163336342344337027E-14, 3.469446951953614189E-14, -3.000000000000002665 ) ) ;
#18151 = ADVANCED_FACE ( 'NONE', ( #12377 ), #17804, .T. ) ;
#18152 = CARTESIAN_POINT ( 'NONE',  ( -64.00000000000045475, 6.245004513516505540E-14, -1.999999999999974021 ) ) ;
#18153 = EDGE_CURVE ( 'NONE', #15246, #3085, #3568, .T. ) ;
#18154 = CARTESIAN_POINT ( 'NONE',  ( 6.495190528383244732, 4.999999999999935163, 3.750000000000003553 ) ) ;
#18155 = CARTESIAN_POINT ( 'NONE',  ( 7.568268608012000520, -0.4673147976723873165, 8.579161250779968384 ) ) ;
#18156 = ORIENTED_EDGE ( 'NONE', *, *, #22185, .T. ) ;
#18158 = ORIENTED_EDGE ( 'NONE', *, *, #14592, .F. ) ;
#18157 = ORIENTED_EDGE ( 'NONE', *, *, #8881, .T. ) ;
#18159 = VERTEX_POINT ( 'NONE', #9778 ) ;
#18160 = CIRCLE ( 'NONE', #20042, 0.2500000000000002220 ) ;
#18162 = ORIENTED_EDGE ( 'NONE', *, *, #9226, .F. ) ;
#18161 = EDGE_LOOP ( 'NONE', ( #16145, #4891, #22144, #16603 ) ) ;
#18163 = CIRCLE ( 'NONE', #8388, 0.5000000000000028866 ) ;
#18164 = B_SPLINE_CURVE_WITH_KNOTS ( 'NONE', 3,
 ( #2984, #4381, #9930, #18631 ),
 .UNSPECIFIED., .F., .F.,
 ( 4, 4 ),
 ( 2.380737581852663157E-07, 0.002336974151641522165 ),
 .UNSPECIFIED. ) ;
#18166 = ORIENTED_EDGE ( 'NONE', *, *, #2185, .T. ) ;
#18165 = ADVANCED_FACE ( 'NONE', ( #18379 ), #7662, .T. ) ;
#18167 = TOROIDAL_SURFACE ( 'NONE', #11398, 6.500000000000000888, 0.5000000000000000000 ) ;
#18168 = CYLINDRICAL_SURFACE ( 'NONE', #22278, 4.000000000000045297 ) ;
#18169 = AXIS2_PLACEMENT_3D ( 'NONE', #3339, #14150, #3445 ) ;
#18170 = EDGE_CURVE ( 'NONE', #7709, #8906, #14795, .T. ) ;
#18171 = EDGE_LOOP ( 'NONE', ( #10690, #16794, #8845, #16055, #5549, #9676 ) ) ;
#18172 = AXIS2_PLACEMENT_3D ( 'NONE', #19394, #10340, #7177 ) ;
#18173 = EDGE_LOOP ( 'NONE', ( #14509, #12180, #4367, #3714 ) ) ;
#18174 = AXIS2_PLACEMENT_3D ( 'NONE', #8007, #22241, #15284 ) ;
#18175 = ADVANCED_FACE ( 'NONE', ( #21906 ), #11073, .T. ) ;
#18176 = LINE ( 'NONE', #285, #10314 ) ;
#18177 = EDGE_CURVE ( 'NONE', #7694, #10905, #21612, .T. ) ;
#18178 = DIRECTION ( 'NONE',  ( 7.860214984770699307E-18, -1.409037165336591006E-16, -1.000000000000000000 ) ) ;
#18179 = DIRECTION ( 'NONE',  ( -1.134196829589822059E-15, -6.741645191078037727E-32, 1.000000000000000000 ) ) ;
#18180 = CARTESIAN_POINT ( 'NONE',  ( 61.48996577904083694, -5.119475911334187224, 6.500000000000130562 ) ) ;
#18181 = CARTESIAN_POINT ( 'NONE',  ( 30.00000000029184832, -0.5000000009961480529, -41.54999999999999716 ) ) ;
#18182 = CARTESIAN_POINT ( 'NONE',  ( 7.000000000000006217, -5.999999999999981348, 6.250000000000005329 ) ) ;
#18183 = EDGE_CURVE ( 'NONE', #3915, #19657, #11301, .T. ) ;
#18184 = DIRECTION ( 'NONE',  ( -0.6819983600625061371, -0.7313537016191633544, 0.000000000000000000 ) ) ;
#18185 = DIRECTION ( 'NONE',  ( 0.000000000000000000, 0.000000000000000000, 1.000000000000000000 ) ) ;
#18186 = CIRCLE ( 'NONE', #6916, 3.300000000000019806 ) ;
#18187 = EDGE_CURVE ( 'NONE', #4163, #17239, #5354, .T. ) ;
#18188 = AXIS2_PLACEMENT_3D ( 'NONE', #2336, #21993, #9520 ) ;
#18189 = DIRECTION ( 'NONE',  ( 1.000000000000000000, 0.000000000000000000, 0.000000000000000000 ) ) ;
#18190 = CIRCLE ( 'NONE', #11030, 2.550000000000010481 ) ;
#18191 = CARTESIAN_POINT ( 'NONE',  ( 37.04362427881598308, 10.78777973366386078, -2.545175158707025265 ) ) ;
#18192 = AXIS2_PLACEMENT_3D ( 'NONE', #10318, #8559, #17968 ) ;
#18193 = EDGE_CURVE ( 'NONE', #6496, #5349, #2419, .T. ) ;
#18194 = ORIENTED_EDGE ( 'NONE', *, *, #17314, .T. ) ;
#18195 = DIRECTION ( 'NONE',  ( -3.330669073875432643E-16, -4.437342591868153746E-31, 1.000000000000000000 ) ) ;
#18197 = VERTEX_POINT ( 'NONE', #6024 ) ;
#18196 = EDGE_LOOP ( 'NONE', ( #2994, #17751, #11040, #12158 ) ) ;
#18198 = EDGE_LOOP ( 'NONE', ( #8058, #15345, #17602, #12041 ) ) ;
#18199 = ORIENTED_EDGE ( 'NONE', *, *, #2887, .F. ) ;
#18200 = ORIENTED_EDGE ( 'NONE', *, *, #19668, .F. ) ;
#18201 = ORIENTED_EDGE ( 'NONE', *, *, #17085, .T. ) ;
#18202 = DIRECTION ( 'NONE',  ( -1.000000000000000000, 5.055479844275211845E-14, -3.717264591378832268E-16 ) ) ;
#18203 = AXIS2_PLACEMENT_3D ( 'NONE', #14498, #23223, #9204 ) ;
#18204 = CYLINDRICAL_SURFACE ( 'NONE', #21532, 6.000000000000000000 ) ;
#18205 = AXIS2_PLACEMENT_3D ( 'NONE', #3465, #15579, #21365 ) ;
#18206 = CARTESIAN_POINT ( 'NONE',  ( 4.175075985190096262, -2.060370777630153416, -3.568666869285546994 ) ) ;
#18207 = DIRECTION ( 'NONE',  ( 2.172745813409349776E-17, -1.000000000000000000, 1.309377075419428048E-16 ) ) ;
#18208 = DIRECTION ( 'NONE',  ( 0.000000000000000000, 0.000000000000000000, -1.000000000000000000 ) ) ;
#18209 = EDGE_CURVE ( 'NONE', #23148, #9224, #6506, .T. ) ;
#18210 = CYLINDRICAL_SURFACE ( 'NONE', #2111, 0.5000000000000004441 ) ;
#18211 = CARTESIAN_POINT ( 'NONE',  ( 54.42435809754108078, -4.000000000000003553, 6.500000000000081712 ) ) ;
#18212 = LINE ( 'NONE', #328, #16431 ) ;
#18213 = DIRECTION ( 'NONE',  ( -7.395570986446975166E-31, -3.382522293539642681E-32, -1.000000000000000000 ) ) ;
#18214 = LINE ( 'NONE', #16764, #8884 ) ;
#18215 = EDGE_CURVE ( 'NONE', #4366, #13948, #3900, .T. ) ;
#18216 = CIRCLE ( 'NONE', #12182, 0.5000000000000022204 ) ;
#18217 = DIRECTION ( 'NONE',  ( 9.693647360340828445E-26, 0.000000000000000000, -1.000000000000000000 ) ) ;
#18218 = FACE_OUTER_BOUND ( 'NONE', #18969, .T. ) ;
#18219 = EDGE_LOOP ( 'NONE', ( #2728, #7804, #5163, #6299 ) ) ;
#18220 = ORIENTED_EDGE ( 'NONE', *, *, #13783, .F. ) ;
#18221 = CARTESIAN_POINT ( 'NONE',  ( -6.958039891257955745, 36.00029345514013102, -26.50000000000000000 ) ) ;
#18222 = FACE_OUTER_BOUND ( 'NONE', #20839, .T. ) ;
#18223 = EDGE_LOOP ( 'NONE', ( #14428, #8693, #6031, #11216 ) ) ;
#18224 = CARTESIAN_POINT ( 'NONE',  ( -5.350349885510485848, 36.24720445779466615, -18.90862932150717413 ) ) ;
#18225 = DIRECTION ( 'NONE',  ( 1.000000000000000000, 3.254448077276381206E-32, 1.066788928082016908E-26 ) ) ;
#18226 = CARTESIAN_POINT ( 'NONE',  ( 3.950241966887857004, -2.668221755853800392, -2.378504353000562066 ) ) ;
#18227 = DIRECTION ( 'NONE',  ( -2.172745813409349776E-17, 1.000000000000000000, -1.309377075419428048E-16 ) ) ;
#18228 = CARTESIAN_POINT ( 'NONE',  ( 36.00000000029184832, 2.999999999003851503, -39.00000000000000000 ) ) ;
#18229 = VERTEX_POINT ( 'NONE', #18259 ) ;
#18230 = DIRECTION ( 'NONE',  ( 1.000000000000000000, 0.000000000000000000, 0.000000000000000000 ) ) ;
#18231 = CARTESIAN_POINT ( 'NONE',  ( -4.024497503033626522, -2.323544716729399884, -3.572167766733401528 ) ) ;
#18232 = DIRECTION ( 'NONE',  ( -1.066786462891689527E-26, -6.656013887802287108E-31, -1.000000000000000000 ) ) ;
#18233 = CARTESIAN_POINT ( 'NONE',  ( -6.999999999708142795, 38.99999999900385461, -18.50000000000000355 ) ) ;
#18234 = DIRECTION ( 'NONE',  ( -1.333893503340774882E-15, -2.778352770573747380E-17, -1.000000000000000000 ) ) ;
#18235 = CYLINDRICAL_SURFACE ( 'NONE', #4030, 0.5000000000000038858 ) ;
#18236 = PLANE ( 'NONE',  #553 ) ;
#18237 = DIRECTION ( 'NONE',  ( -0.000000000000000000, -0.000000000000000000, 1.000000000000000000 ) ) ;
#18238 = CARTESIAN_POINT ( 'NONE',  ( 37.86602540378459025, -1.387778780781445676E-14, -2.133974596215476360 ) ) ;
#18239 = DIRECTION ( 'NONE',  ( -1.000000000000000000, -1.910522504832140594E-31, 5.551115123125818447E-17 ) ) ;
#18240 = APPLICATION_PROTOCOL_DEFINITION ( 'draft international standard', 'automotive_design', 1998, #18699 ) ;
#18241 = CIRCLE ( 'NONE', #1342, 2.549999999999997158 ) ;
#18242 = ORIENTED_EDGE ( 'NONE', *, *, #11532, .T. ) ;
#18243 = EDGE_CURVE ( 'NONE', #14311, #2294, #10625, .T. ) ;
#18244 = EDGE_LOOP ( 'NONE', ( #21265, #10063, #1807, #14164 ) ) ;
#18246 = ORIENTED_EDGE ( 'NONE', *, *, #21101, .T. ) ;
#18245 = ORIENTED_EDGE ( 'NONE', *, *, #7013, .T. ) ;
#18247 = EDGE_CURVE ( 'NONE', #12125, #16865, #496, .T. ) ;
#18248 = CARTESIAN_POINT ( 'NONE',  ( 66.26395429947837101, -4.000000000000003553, 6.500000000000110134 ) ) ;
#18249 = CARTESIAN_POINT ( 'NONE',  ( 37.60054931026179759, 0.05202134937413122051, -2.399450689738933384 ) ) ;
#18250 = CARTESIAN_POINT ( 'NONE',  ( 8.037202331403122457, -11.80340871766173017, 7.528743044528821926 ) ) ;
#18251 = CARTESIAN_POINT ( 'NONE',  ( -7.491585531133571507, -11.85620892266377702, 7.320610673787158795 ) ) ;
#18252 = DIRECTION ( 'NONE',  ( -0.6819983600625060260, -0.7313537016191635765, -6.106365041599011361E-16 ) ) ;
#18253 = DIRECTION ( 'NONE',  ( 0.000000000000000000, 0.000000000000000000, 1.000000000000000000 ) ) ;
#18254 = CARTESIAN_POINT ( 'NONE',  ( -6.226186441994415510, 36.09747688189035841, -16.97411279881559310 ) ) ;
#18255 = CARTESIAN_POINT ( 'NONE',  ( 124.5000000000019469, -13.52760560296373171, -6.938893903907228378E-15 ) ) ;
#18256 = CARTESIAN_POINT ( 'NONE',  ( 3.191783008269916344, 1.561572887838375445, -3.971669662941486045 ) ) ;
#18257 = B_SPLINE_CURVE_WITH_KNOTS ( 'NONE', 3,
 ( #11640, #4004, #2702, #22126, #20255, #7663, #13188, #16574, #16471, #20360, #726, #7547, #6131, #11185, #13309, #20489 ),
 .UNSPECIFIED., .F., .F.,
 ( 4, 3, 3, 3, 3, 4 ),
 ( 0.000000000000000000, 3.315506744709154877E-05, 6.608280158698813327E-05, 0.0001026520855291333285, 0.0001376952025664795293, 0.0001398064759190609924 ),
 .UNSPECIFIED. ) ;
#18258 = CARTESIAN_POINT ( 'NONE',  ( 4.000000000000003553, 1.557668341133516599, -5.440303434304243346 ) ) ;
#18259 = CARTESIAN_POINT ( 'NONE',  ( 4.175813232069142344, -2.061359961916371830, -3.570380186727398986 ) ) ;
#18260 =( NAMED_UNIT ( * ) PLANE_ANGLE_UNIT ( ) SI_UNIT ( $, .RADIAN. ) );
#18261 = DIRECTION ( 'NONE',  ( -1.000000000000000000, -2.699383410053119644E-30, -3.330669073875432643E-16 ) ) ;
#18262 = CONICAL_SURFACE ( 'NONE', #11496, 4.000000000000022204, 0.8911886515913840512 ) ;
#18263 = DIRECTION ( 'NONE',  ( 1.000000000000000000, -7.477632011778292156E-48, 3.885780586188017323E-16 ) ) ;
#18264 = CARTESIAN_POINT ( 'NONE',  ( 3.999999999999937828, -1.560351142792990142, -0.2242961665059441667 ) ) ;
#18265 = CARTESIAN_POINT ( 'NONE',  ( 7.796097383573778572, -0.6999727310043983852, 7.943830786858195658 ) ) ;
#18266 = VERTEX_POINT ( 'NONE', #16479 ) ;
#18268 = ORIENTED_EDGE ( 'NONE', *, *, #6153, .F. ) ;
#18267 = ORIENTED_EDGE ( 'NONE', *, *, #14126, .F. ) ;
#18269 = ADVANCED_FACE ( 'NONE', ( #7555 ), #20139, .T. ) ;
#18270 = ORIENTED_EDGE ( 'NONE', *, *, #13956, .F. ) ;
#18272 = ORIENTED_EDGE ( 'NONE', *, *, #5238, .T. ) ;
#18271 = VERTEX_POINT ( 'NONE', #11530 ) ;
#18273 = VECTOR ( 'NONE', #2891, 1000.000000000000000 ) ;
#18274 = ORIENTED_EDGE ( 'NONE', *, *, #14291, .T. ) ;
#18275 = CARTESIAN_POINT ( 'NONE',  ( 59.19834661797866460, 1.119475911334100182, 6.500000000000130562 ) ) ;
#18276 = ORIENTED_EDGE ( 'NONE', *, *, #5616, .F. ) ;
#18277 = VERTEX_POINT ( 'NONE', #11421 ) ;
#18278 = CARTESIAN_POINT ( 'NONE',  ( -8.658472430787128582E-13, 0.6000000000000130784, 3.228722604634005844 ) ) ;
#18279 = ADVANCED_FACE ( 'NONE', ( #2367 ), #18581, .T. ) ;
#18280 = VECTOR ( 'NONE', #5992, 1000.000000000000000 ) ;
#18281 = EDGE_CURVE ( 'NONE', #7570, #15190, #22665, .T. ) ;
#18282 = CARTESIAN_POINT ( 'NONE',  ( -6.938893903907228378E-14, -4.618802153517121312, -3.433295621305409107 ) ) ;
#18283 = FACE_OUTER_BOUND ( 'NONE', #12853, .T. ) ;
#18284 = EDGE_CURVE ( 'NONE', #9593, #19900, #4460, .T. ) ;
#18285 = CARTESIAN_POINT ( 'NONE',  ( -9.714451465470119729E-14, 1.999999999999890754, 8.000000000000090594 ) ) ;
#18286 = AXIS2_PLACEMENT_3D ( 'NONE', #12641, #16743, #2288 ) ;
#18287 = DIRECTION ( 'NONE',  ( 1.000000000000000000, -4.190823558986610327E-31, 1.733449886265890494E-32 ) ) ;
#18288 = LINE ( 'NONE', #18515, #3341 ) ;
#18289 = CARTESIAN_POINT ( 'NONE',  ( -66.55000000000039506, -3.200000000000081002, -2.000000000000029310 ) ) ;
#18290 = DIRECTION ( 'NONE',  ( 1.333893503340774882E-15, 2.778352770573747380E-17, 1.000000000000000000 ) ) ;
#18291 = CARTESIAN_POINT ( 'NONE',  ( 37.77870956205639885, 11.00000000000000000, -2.308606279672897887 ) ) ;
#18292 = ORIENTED_EDGE ( 'NONE', *, *, #333, .F. ) ;
#18293 = EDGE_CURVE ( 'NONE', #8517, #21954, #9563, .T. ) ;
#18294 = EDGE_CURVE ( 'NONE', #13948, #13984, #2709, .T. ) ;
#18295 = VECTOR ( 'NONE', #16608, 1000.000000000000000 ) ;
#18296 = CARTESIAN_POINT ( 'NONE',  ( 77.42435809754141474, -6.499999999999811706, 6.000000000000095923 ) ) ;
#18298 = EDGE_LOOP ( 'NONE', ( #22362, #10001, #3119 ) ) ;
#18297 = VERTEX_POINT ( 'NONE', #19183 ) ;
#18299 = AXIS2_PLACEMENT_3D ( 'NONE', #13551, #18724, #1095 ) ;
#18300 = ORIENTED_EDGE ( 'NONE', *, *, #13863, .T. ) ;
#18301 = CIRCLE ( 'NONE', #661, 0.7499999999999997780 ) ;
#18302 = EDGE_LOOP ( 'NONE', ( #10168, #19700, #21465 ) ) ;
#18303 = VERTEX_POINT ( 'NONE', #20609 ) ;
#18304 = AXIS2_PLACEMENT_3D ( 'NONE', #16930, #21162, #6371 ) ;
#18305 = EDGE_CURVE ( 'NONE', #8962, #888, #18950, .T. ) ;
#18306 = EDGE_LOOP ( 'NONE', ( #271, #13672, #19346, #10860 ) ) ;
#18307 = FACE_OUTER_BOUND ( 'NONE', #16142, .T. ) ;
#18308 = VECTOR ( 'NONE', #15736, 1000.000000000000000 ) ;
#18309 = EDGE_CURVE ( 'NONE', #5263, #9570, #17056, .T. ) ;
#18310 = CARTESIAN_POINT ( 'NONE',  ( 88.75737332930583534, -11.02760560296348125, -6.500000000000047073 ) ) ;
#18311 = EDGE_CURVE ( 'NONE', #4916, #16377, #2795, .T. ) ;
#18312 = LINE ( 'NONE', #2190, #3466 ) ;
#18313 = FACE_OUTER_BOUND ( 'NONE', #11693, .T. ) ;
#18314 = CARTESIAN_POINT ( 'NONE',  ( 35.50000000029184832, -9.961476088449217059E-10, -26.50000000000000000 ) ) ;
#18315 = AXIS2_PLACEMENT_3D ( 'NONE', #874, #11675, #11799 ) ;
#18316 = DIRECTION ( 'NONE',  ( 0.000000000000000000, 1.000000000000000000, 0.000000000000000000 ) ) ;
#18317 = CIRCLE ( 'NONE', #4396, 3.499999999999995115 ) ;
#18318 = CARTESIAN_POINT ( 'NONE',  ( -2.500000000000002220, 0.000000000000000000, -5.574599999999999334 ) ) ;
#18319 = CARTESIAN_POINT ( 'NONE',  ( 1.040834085586084257E-14, 1.500000000000029088, -17.00000000000000711 ) ) ;
#18320 = CARTESIAN_POINT ( 'NONE',  ( 7.884991313526934498, -1.682691736113213432, 7.773664271103622347 ) ) ;
#18321 = AXIS2_PLACEMENT_3D ( 'NONE', #21429, #1756, #12808 ) ;
#18322 = DIRECTION ( 'NONE',  ( 1.000000000000000000, 4.252453317207022018E-31, -5.551115123125818447E-17 ) ) ;
#18323 = VECTOR ( 'NONE', #19562, 1000.000000000000000 ) ;
#18324 = ADVANCED_FACE ( 'NONE', ( #13889 ), #6375, .T. ) ;
#18325 = SURFACE_SIDE_STYLE ('',( #11479 ) ) ;
#18326 = CARTESIAN_POINT ( 'NONE',  ( -65.55642023346347003, -8.326672684688674053E-14, -11.87813525200320797 ) ) ;
#18327 = CONICAL_SURFACE ( 'NONE', #7074, 4.750000000000000888, 1.047197551196600074 ) ;
#18328 = VERTEX_POINT ( 'NONE', #8253 ) ;
#18329 = AXIS2_PLACEMENT_3D ( 'NONE', #20828, #3727, #6929 ) ;
#18330 = EDGE_CURVE ( 'NONE', #3791, #15286, #19068, .T. ) ;
#18331 = AXIS2_PLACEMENT_3D ( 'NONE', #17209, #6522, #2516 ) ;
#18332 = CARTESIAN_POINT ( 'NONE',  ( 10.50000000000000888, -1.999999999999984457, 6.250000000000005329 ) ) ;
#18333 = CARTESIAN_POINT ( 'NONE',  ( -56.91911807125098477, -3.200000000000108979, -8.333333333333413862 ) ) ;
#18334 = ORIENTED_EDGE ( 'NONE', *, *, #18462, .F. ) ;
#18335 = AXIS2_PLACEMENT_3D ( 'NONE', #8330, #2922, #1391 ) ;
#18336 = DIRECTION ( 'NONE',  ( 1.000000000000000000, 1.479114197289387852E-30, -2.013525853228518840E-32 ) ) ;
#18337 = CARTESIAN_POINT ( 'NONE',  ( 0.000000000000000000, 0.000000000000000000, 3.469446951953614189E-15 ) ) ;
#18338 = CARTESIAN_POINT ( 'NONE',  ( 8.954763739086823549, -0.5000000000000004441, 6.678571428571450141 ) ) ;
#18339 = DIRECTION ( 'NONE',  ( 1.550910762415566494E-16, 1.000000000000000000, -8.135128085091684243E-31 ) ) ;
#18340 = CARTESIAN_POINT ( 'NONE',  ( 0.000000000000000000, 0.000000000000000000, -3.499999999999996003 ) ) ;
#18341 = AXIS2_PLACEMENT_3D ( 'NONE', #22843, #13893, #3201 ) ;
#18342 = CARTESIAN_POINT ( 'NONE',  ( 73.50000000000116529, -13.52760560296348302, 3.469446951953614189E-14 ) ) ;
#18343 = AXIS2_PLACEMENT_3D ( 'NONE', #5539, #9181, #14005 ) ;
#18344 = CARTESIAN_POINT ( 'NONE',  ( -10.49999999999996803, -0.5000000000000004441, 9.250000000000035527 ) ) ;
#18345 = CARTESIAN_POINT ( 'NONE',  ( 2.775557561562891351E-14, 10.75000000000000000, -10.43301270189220276 ) ) ;
#18346 = FACE_OUTER_BOUND ( 'NONE', #19545, .T. ) ;
#18347 = CARTESIAN_POINT ( 'NONE',  ( -10.49999999999998224, -0.5000000000000038858, 5.750000000000032863 ) ) ;
#18348 = CARTESIAN_POINT ( 'NONE',  ( 124.5000000000019185, -7.000000000000062172, -5.999999999999984901 ) ) ;
#18349 = B_SPLINE_CURVE_WITH_KNOTS ( 'NONE', 3,
 ( #2506, #5177, #7183, #22954 ),
 .UNSPECIFIED., .F., .F.,
 ( 4, 4 ),
 ( 0.004330357959029877170, 0.008660484977952064359 ),
 .UNSPECIFIED. ) ;
#18350 = DIRECTION ( 'NONE',  ( 1.000000000000000000, -1.276756478318922922E-15, 1.342094922251465017E-15 ) ) ;
#18351 = CYLINDRICAL_SURFACE ( 'NONE', #13475, 0.4999999999999978351 ) ;
#18352 = SURFACE_STYLE_FILL_AREA ( #3988 ) ;
#18353 = PRESENTATION_LAYER_ASSIGNMENT (  '', '', ( #5203 ) ) ;
#18354 = CARTESIAN_POINT ( 'NONE',  ( 3.961551342854305435, -2.319461885623339548, -2.982574167880875926 ) ) ;
#18355 = AXIS2_PLACEMENT_3D ( 'NONE', #6249, #18827, #14943 ) ;
#18356 = ADVANCED_FACE ( 'NONE', ( #17288 ), #16625, .T. ) ;
#18357 = AXIS2_PLACEMENT_3D ( 'NONE', #21976, #18664, #798 ) ;
#18358 = SHAPE_DEFINITION_REPRESENTATION ( #1609, #15574 ) ;
#18359 = AXIS2_PLACEMENT_3D ( 'NONE', #1290, #13522, #22701 ) ;
#18360 = ORIENTED_EDGE ( 'NONE', *, *, #4321, .F. ) ;
#18361 = EDGE_CURVE ( 'NONE', #4169, #4164, #13545, .T. ) ;
#18363 = EDGE_LOOP ( 'NONE', ( #2276, #20411, #8002, #16348 ) ) ;
#18362 = ORIENTED_EDGE ( 'NONE', *, *, #9240, .F. ) ;
#18364 = APPLICATION_CONTEXT ( 'automotive_design' ) ;
#18365 = DIRECTION ( 'NONE',  ( 5.551115123125782702E-16, 1.201780285297635172E-31, -1.000000000000000000 ) ) ;
#18366 = EDGE_CURVE ( 'NONE', #16716, #902, #9802, .T. ) ;
#18367 = STYLED_ITEM ( 'NONE', ( #13945 ), #19561 ) ;
#18368 = CARTESIAN_POINT ( 'NONE',  ( 37.43301270189237329, 0.2499999999999700795, -2.999999999999904077 ) ) ;
#18369 = CARTESIAN_POINT ( 'NONE',  ( 8.422565759993609902, -12.00000000000004796, 6.396710472006761350 ) ) ;
#18370 = CARTESIAN_POINT ( 'NONE',  ( -3.937547562846346327, -0.7499999999999433786, -2.974837901130639395 ) ) ;
#18371 = VECTOR ( 'NONE', #15638, 1000.000000000000114 ) ;
#18372 = LINE ( 'NONE', #11186, #20314 ) ;
#18373 = FACE_OUTER_BOUND ( 'NONE', #15755, .T. ) ;
#18374 = CARTESIAN_POINT ( 'NONE',  ( -3.529586291208667935E-15, -0.5999999999999897637, -3.228048788193013774 ) ) ;
#18375 = VECTOR ( 'NONE', #21495, 1000.000000000000000 ) ;
#18376 = FACE_OUTER_BOUND ( 'NONE', #6414, .T. ) ;
#18377 = CIRCLE ( 'NONE', #5608, 2.500000000000006661 ) ;
#18378 = CARTESIAN_POINT ( 'NONE',  ( 77.42435809754137210, -6.999999999999811706, 6.500000000000081712 ) ) ;
#18379 = FACE_OUTER_BOUND ( 'NONE', #20422, .T. ) ;
#18380 = SURFACE_STYLE_FILL_AREA ( #11194 ) ;
#18381 = DIRECTION ( 'NONE',  ( 0.000000000000000000, 0.000000000000000000, -1.000000000000000000 ) ) ;
#18382 = CARTESIAN_POINT ( 'NONE',  ( 6.999999999999978684, -3.018576030000261312, 8.916666666666724694 ) ) ;
#18383 = LINE ( 'NONE', #9440, #18695 ) ;
#18384 = CARTESIAN_POINT ( 'NONE',  ( 7.694134585029391182, -0.3119908745745466616, 8.172315317060892426 ) ) ;
#18385 = EDGE_LOOP ( 'NONE', ( #7653, #16869 ) ) ;
#18386 = PRESENTATION_STYLE_ASSIGNMENT (( #19924 ) ) ;
#18388 = ORIENTED_EDGE ( 'NONE', *, *, #12245, .T. ) ;
#18387 = ORIENTED_EDGE ( 'NONE', *, *, #7948, .F. ) ;
#18389 = ORIENTED_EDGE ( 'NONE', *, *, #18965, .T. ) ;
#18391 = ORIENTED_EDGE ( 'NONE', *, *, #10217, .T. ) ;
#18390 = ORIENTED_EDGE ( 'NONE', *, *, #472, .F. ) ;
#18392 = ORIENTED_EDGE ( 'NONE', *, *, #20056, .F. ) ;
#18393 = DIRECTION ( 'NONE',  ( -0.6819983600624981435, -0.7313537016191709039, 0.000000000000000000 ) ) ;
#18394 = EDGE_LOOP ( 'NONE', ( #34, #5926, #22852, #17747 ) ) ;
#18395 = ORIENTED_EDGE ( 'NONE', *, *, #13361, .T. ) ;
#18396 = DIRECTION ( 'NONE',  ( 8.659560563109223167E-17, -0.7071067811865516806, 0.7071067811865434649 ) ) ;
#18397 = CARTESIAN_POINT ( 'NONE',  ( -45.01801948466080461, -6.474873734152955862, 7.500000000000062172 ) ) ;
#18398 = DIRECTION ( 'NONE',  ( 1.550910762415566494E-16, 1.000000000000000000, -8.135128085091684243E-31 ) ) ;
#18399 = AXIS2_PLACEMENT_3D ( 'NONE', #10244, #5308, #14014 ) ;
#18400 = CARTESIAN_POINT ( 'NONE',  ( -7.602880770961763623, -2.006500808705121486, 8.461619612152039949 ) ) ;
#18401 = PRODUCT_DEFINITION ( 'UNKNOWN', '', #14638, #11918 ) ;
#18402 = CARTESIAN_POINT ( 'NONE',  ( 4.165266963751727225, -2.049631966911998671, -3.550066703508907295 ) ) ;
#18403 = DIRECTION ( 'NONE',  ( -3.885780586188016830E-16, -4.437342591868156373E-31, 1.000000000000000000 ) ) ;
#18404 = DIRECTION ( 'NONE',  ( -3.070652698126927723E-17, -1.000000000000000000, 4.167305704548413124E-17 ) ) ;
#18405 = LINE ( 'NONE', #9811, #16217 ) ;
#18406 = EDGE_CURVE ( 'NONE', #20542, #13382, #15125, .T. ) ;
#18407 = CARTESIAN_POINT ( 'NONE',  ( 0.000000000000000000, 0.000000000000000000, -3.499999999999996003 ) ) ;
#18408 = CARTESIAN_POINT ( 'NONE',  ( 37.45482484129320255, 10.78777973366397092, -2.956375721184426819 ) ) ;
#18409 = ORIENTED_EDGE ( 'NONE', *, *, #20155, .F. ) ;
#18410 = ADVANCED_FACE ( 'NONE', ( #10015 ), #21601, .T. ) ;
#18411 = CARTESIAN_POINT ( 'NONE',  ( -1.734723475976807094E-14, 2.000000000000001776, -17.75000000000000711 ) ) ;
#18413 = ORIENTED_EDGE ( 'NONE', *, *, #19893, .F. ) ;
#18412 = ORIENTED_EDGE ( 'NONE', *, *, #12002, .T. ) ;
#18414 = VERTEX_POINT ( 'NONE', #8132 ) ;
#18415 = EDGE_LOOP ( 'NONE', ( #2291, #8604, #632, #5050, #9048, #14052 ) ) ;
#18416 = EDGE_CURVE ( 'NONE', #18645, #15578, #17384, .T. ) ;
#18417 = ORIENTED_EDGE ( 'NONE', *, *, #18284, .F. ) ;
#18418 = ORIENTED_EDGE ( 'NONE', *, *, #19543, .T. ) ;
#18419 = EDGE_LOOP ( 'NONE', ( #7791, #22647, #22209 ) ) ;
#18420 = DIRECTION ( 'NONE',  ( -1.000000000000000000, 4.190823558986610327E-31, -1.733449886265890494E-32 ) ) ;
#18421 = CARTESIAN_POINT ( 'NONE',  ( 0.000000000000000000, -11.33467790002633180, -1.387778780781445676E-14 ) ) ;
#18422 = CARTESIAN_POINT ( 'NONE',  ( 66.26395429947839943, 0.000000000000000000, 6.000000000000178524 ) ) ;
#18423 = EDGE_CURVE ( 'NONE', #15911, #21123, #22487, .T. ) ;
#18424 = LINE ( 'NONE', #2191, #5745 ) ;
#18425 = DIRECTION ( 'NONE',  ( -0.7071067811865491270, -0.7071067811865461294, -1.565905175853767167E-16 ) ) ;
#18426 = VECTOR ( 'NONE', #8617, 1000.000000000000114 ) ;
#18427 = PLANE ( 'NONE',  #8334 ) ;
#18428 = CARTESIAN_POINT ( 'NONE',  ( -8.260108127873365902, -11.89083139210929296, 7.249251683976637217 ) ) ;
#18429 = ADVANCED_FACE ( 'NONE', ( #17172 ), #1315, .F. ) ;
#18430 = CARTESIAN_POINT ( 'NONE',  ( -7.525553787417716300, -12.92907334721332013, 8.786654903594138588 ) ) ;
#18431 = LINE ( 'NONE', #16652, #22883 ) ;
#18432 = DIRECTION ( 'NONE',  ( 1.000000000000000000, 1.479114197289397135E-31, 5.916456789157588541E-31 ) ) ;
#18433 = CARTESIAN_POINT ( 'NONE',  ( -50.65685424949274562, -3.200000000000091660, 8.000000000000062172 ) ) ;
#18434 = ADVANCED_FACE ( 'NONE', ( #22721 ), #6718, .T. ) ;
#18435 = ADVANCED_BREP_SHAPE_REPRESENTATION ( '', ( #12837, #22115 ), #7836 ) ;
#18436 = FACE_OUTER_BOUND ( 'NONE', #6589, .T. ) ;
#18437 = CARTESIAN_POINT ( 'NONE',  ( 2.918498775983380256E-10, 6.999999999003851947, -19.00000000000000355 ) ) ;
#18438 = ADVANCED_FACE ( 'NONE', ( #8835 ), #12503, .F. ) ;
#18439 = EDGE_CURVE ( 'NONE', #1775, #5689, #11805, .T. ) ;
#18440 = AXIS2_PLACEMENT_3D ( 'NONE', #4823, #10230, #17399 ) ;
#18441 = VERTEX_POINT ( 'NONE', #7309 ) ;
#18442 = CARTESIAN_POINT ( 'NONE',  ( 6.000000000291855429, 2.999999999003851503, -5.999999999999998224 ) ) ;
#18443 = PLANE ( 'NONE',  #6459 ) ;
#18444 = ORIENTED_EDGE ( 'NONE', *, *, #3922, .T. ) ;
#18445 = CARTESIAN_POINT ( 'NONE',  ( 112.6756160111034575, -11.28140466348828674, -6.500000000000040856 ) ) ;
#18446 = LINE ( 'NONE', #2447, #10752 ) ;
#18447 = EDGE_CURVE ( 'NONE', #19838, #7684, #23193, .T. ) ;
#18448 = CARTESIAN_POINT ( 'NONE',  ( 5.484827557301438894, 1.749999999999998002, -2.775557561562891351E-14 ) ) ;
#18449 = CARTESIAN_POINT ( 'NONE',  ( 24.75000000000000355, 2.000000000000029310, -2.000000000000005329 ) ) ;
#18450 = EDGE_CURVE ( 'NONE', #1694, #5384, #15508, .T. ) ;
#18451 = ADVANCED_FACE ( 'NONE', ( #15761 ), #5391, .T. ) ;
#18452 = DIRECTION ( 'NONE',  ( -3.885780586188016830E-16, -4.437342591868156373E-31, 1.000000000000000000 ) ) ;
#18453 = CARTESIAN_POINT ( 'NONE',  ( 86.02937988905580369, -9.453020409440155092, -6.499999999999943157 ) ) ;
#18454 = CARTESIAN_POINT ( 'NONE',  ( 2.498001805406602216E-13, 3.000000000000002665, 6.500000000000103029 ) ) ;
#18455 = LINE ( 'NONE', #2226, #10647 ) ;
#18456 = CARTESIAN_POINT ( 'NONE',  ( -1.387778780781445676E-14, 2.000000000000001776, -1.500000000000001332 ) ) ;
#18457 = CARTESIAN_POINT ( 'NONE',  ( -42.54314575050785407, -4.000000000000021316, 8.000000000000007105 ) ) ;
#18458 = CIRCLE ( 'NONE', #8318, 2.800000000000017586 ) ;
#18459 = AXIS2_PLACEMENT_3D ( 'NONE', #5905, #3597, #17949 ) ;
#18460 = CARTESIAN_POINT ( 'NONE',  ( 3.000000000291852764, 42.99999999900385461, -26.50000000000000000 ) ) ;
#18461 = LINE ( 'NONE', #16452, #5958 ) ;
#18462 = EDGE_CURVE ( 'NONE', #9560, #22731, #12288, .T. ) ;
#18463 = EDGE_CURVE ( 'NONE', #22005, #12160, #13699, .T. ) ;
#18464 = CARTESIAN_POINT ( 'NONE',  ( 4.033901012036569256, -2.321269032827520284, -2.979444097106667577 ) ) ;
#18465 = EDGE_CURVE ( 'NONE', #8438, #19198, #22, .T. ) ;
#18466 = EDGE_LOOP ( 'NONE', ( #13066, #22212, #20098, #12694 ) ) ;
#18467 = CIRCLE ( 'NONE', #17332, 0.2500000000000002220 ) ;
#18469 = ORIENTED_EDGE ( 'NONE', *, *, #22498, .T. ) ;
#18468 = ORIENTED_EDGE ( 'NONE', *, *, #20616, .T. ) ;
#18470 = AXIS2_PLACEMENT_3D ( 'NONE', #11830, #21011, #8537 ) ;
#18471 = AXIS2_PLACEMENT_3D ( 'NONE', #5320, #12239, #5207 ) ;
#18472 = DIRECTION ( 'NONE',  ( 1.733449886265890494E-32, 4.190823558986611203E-31, -1.000000000000000000 ) ) ;
#18473 = CARTESIAN_POINT ( 'NONE',  ( -43.10883117545713361, -4.565685424949256443, -7.500000000000007105 ) ) ;
#18474 = CYLINDRICAL_SURFACE ( 'NONE', #1130, 6.999999999999999112 ) ;
#18475 = ORIENTED_EDGE ( 'NONE', *, *, #16464, .F. ) ;
#18476 = FACE_OUTER_BOUND ( 'NONE', #56, .T. ) ;
#18477 = LINE ( 'NONE', #2360, #6429 ) ;
#18478 = DIRECTION ( 'NONE',  ( -1.000000000000000000, -6.938893903907186568E-15, 0.000000000000000000 ) ) ;
#18479 = CYLINDRICAL_SURFACE ( 'NONE', #20192, 0.5000000000000000000 ) ;
#18480 = DIRECTION ( 'NONE',  ( 3.032184104443272185E-30, 1.000000000000000000, -7.395570986447005381E-32 ) ) ;
#18481 = AXIS2_PLACEMENT_3D ( 'NONE', #16018, #264, #9084 ) ;
#18482 = CARTESIAN_POINT ( 'NONE',  ( 5.600000000000000533, 6.472876824008160606E-16, -5.200000000000004619 ) ) ;
#18483 = DIRECTION ( 'NONE',  ( 1.066811114794977684E-26, 0.000000000000000000, 1.000000000000000000 ) ) ;
#18484 =( LENGTH_UNIT ( ) NAMED_UNIT ( * ) SI_UNIT ( .MILLI., .METRE. ) );
#18485 = CYLINDRICAL_SURFACE ( 'NONE', #8919, 2.500000000000002220 ) ;
#18486 = CARTESIAN_POINT ( 'NONE',  ( -6.866595637047972822, -4.163336342344337027E-14, 27.70872448147272848 ) ) ;
#18487 = LINE ( 'NONE', #5909, #1056 ) ;
#18488 = AXIS2_PLACEMENT_3D ( 'NONE', #22691, #8216, #15833 ) ;
#18489 = CARTESIAN_POINT ( 'NONE',  ( 3.999999999999955147, -2.309401076758532678, -0.5000000000000004441 ) ) ;
#18490 = CARTESIAN_POINT ( 'NONE',  ( -5.484827557301438894, -1.325747111984083793, 0.000000000000000000 ) ) ;
#18491 = AXIS2_PLACEMENT_3D ( 'NONE', #3395, #5147, #17492 ) ;
#18492 = EDGE_CURVE ( 'NONE', #9721, #9717, #19713, .T. ) ;
#18493 = ORIENTED_EDGE ( 'NONE', *, *, #370, .F. ) ;
#18495 = ORIENTED_EDGE ( 'NONE', *, *, #12335, .T. ) ;
#18494 = ORIENTED_EDGE ( 'NONE', *, *, #2403, .F. ) ;
#18496 = ORIENTED_EDGE ( 'NONE', *, *, #7785, .F. ) ;
#18498 = EDGE_LOOP ( 'NONE', ( #9799, #6416 ) ) ;
#18497 = ORIENTED_EDGE ( 'NONE', *, *, #16274, .F. ) ;
#18499 = AXIS2_PLACEMENT_3D ( 'NONE', #2255, #16815, #615 ) ;
#18500 = ORIENTED_EDGE ( 'NONE', *, *, #7385, .F. ) ;
#18501 = CARTESIAN_POINT ( 'NONE',  ( 2.775557561562891351E-14, 10.49999999999999822, -6.499999999999950262 ) ) ;
#18502 = EDGE_LOOP ( 'NONE', ( #13677, #10931, #8963, #4189 ) ) ;
#18503 = ORIENTED_EDGE ( 'NONE', *, *, #3625, .F. ) ;
#18504 = FACE_OUTER_BOUND ( 'NONE', #21475, .T. ) ;
#18505 =( GEOMETRIC_REPRESENTATION_CONTEXT ( 3 ) GLOBAL_UNCERTAINTY_ASSIGNED_CONTEXT ( ( #10963 ) ) GLOBAL_UNIT_ASSIGNED_CONTEXT ( ( #10874, #12638, #18067 ) ) REPRESENTATION_CONTEXT ( 'NONE', 'WORKASPACE' ) );
#18506 = VECTOR ( 'NONE', #20055, 1000.000000000000000 ) ;
#18507 = DIRECTION ( 'NONE',  ( 3.885780586188016830E-16, 4.437342591868156373E-31, -1.000000000000000000 ) ) ;
#18508 = CARTESIAN_POINT ( 'NONE',  ( -42.54314575050793934, -4.000000000000021316, 7.500000000000062172 ) ) ;
#18509 = AXIS2_PLACEMENT_3D ( 'NONE', #2069, #9139, #4068 ) ;
#18510 = CARTESIAN_POINT ( 'NONE',  ( 37.43301270189233776, 10.75000000000000000, -9.999999999999994671 ) ) ;
#18511 = AXIS2_PLACEMENT_3D ( 'NONE', #16157, #6652, #12402 ) ;
#18512 = DIRECTION ( 'NONE',  ( 1.000000000000000000, 1.479114197289388027E-30, -2.013525853228518840E-32 ) ) ;
#18513 = AXIS2_PLACEMENT_3D ( 'NONE', #7397, #20331, #14908 ) ;
#18514 = CARTESIAN_POINT ( 'NONE',  ( 4.175326769692853546, -2.060699556489058448, -3.569236330973427407 ) ) ;
#18515 = CARTESIAN_POINT ( 'NONE',  ( -6.000000000000088818, -7.500000000000007105, 8.000000000000062172 ) ) ;
#18516 = CARTESIAN_POINT ( 'NONE',  ( 4.055498735588670911, -1.410041617599706143, 3.568038744583164057 ) ) ;
#18517 = CYLINDRICAL_SURFACE ( 'NONE', #14820, 0.5000000000000000000 ) ;
#18518 = DIRECTION ( 'NONE',  ( 1.000000000000000000, 0.000000000000000000, 0.000000000000000000 ) ) ;
#18519 = FACE_OUTER_BOUND ( 'NONE', #6160, .T. ) ;
#18520 = VERTEX_POINT ( 'NONE', #3542 ) ;
#18521 = PRODUCT_DEFINITION_CONTEXT ( 'detailed design', #8638, 'design' ) ;
#18522 = VECTOR ( 'NONE', #12463, 1000.000000000000000 ) ;
#18523 = CARTESIAN_POINT ( 'NONE',  ( -55.05572809000125289, 2.700000000000021938, -10.00000000000006395 ) ) ;
#18524 = AXIS2_PLACEMENT_3D ( 'NONE', #12243, #16236, #10497 ) ;
#18526 = ORIENTED_EDGE ( 'NONE', *, *, #6067, .T. ) ;
#18525 = ORIENTED_EDGE ( 'NONE', *, *, #21283, .F. ) ;
#18527 = AXIS2_PLACEMENT_3D ( 'NONE', #20784, #4647, #15460 ) ;
#18528 = CONICAL_SURFACE ( 'NONE', #21552, 2.060000000000013820, 0.9599310885968820317 ) ;
#18529 = VECTOR ( 'NONE', #22616, 1000.000000000000000 ) ;
#18530 = ORIENTED_EDGE ( 'NONE', *, *, #17001, .T. ) ;
#18531 = EDGE_LOOP ( 'NONE', ( #20328, #5923, #12749, #21692, #14650, #1505, #5824 ) ) ;
#18532 = ORIENTED_EDGE ( 'NONE', *, *, #6081, .T. ) ;
#18533 = EDGE_CURVE ( 'NONE', #21802, #6614, #5185, .T. ) ;
#18534 = EDGE_LOOP ( 'NONE', ( #21028, #13520, #13159, #1719 ) ) ;
#18535 = CARTESIAN_POINT ( 'NONE',  ( -6.938893903907228378E-15, -9.999999999999968026, 0.000000000000000000 ) ) ;
#18536 = FACE_OUTER_BOUND ( 'NONE', #11587, .T. ) ;
#18537 = ORIENTED_EDGE ( 'NONE', *, *, #21775, .T. ) ;
#18538 = DIRECTION ( 'NONE',  ( 1.000000000000000000, 2.699383410053119293E-30, 4.336808689941968432E-16 ) ) ;
#18539 = AXIS2_PLACEMENT_3D ( 'NONE', #1060, #20582, #22700 ) ;
#18540 = DIRECTION ( 'NONE',  ( -1.550910762415566494E-16, -1.000000000000000000, 8.135128085091684243E-31 ) ) ;
#18541 = AXIS2_PLACEMENT_3D ( 'NONE', #18930, #16908, #1476 ) ;
#18542 = CARTESIAN_POINT ( 'NONE',  ( 8.660254037844413944, 4.689110867544616035, 2.775557561562891351E-14 ) ) ;
#18543 = CARTESIAN_POINT ( 'NONE',  ( -6.495190528383335327, 5.000000000000018652, -3.750000000000003553 ) ) ;
#18544 = AXIS2_PLACEMENT_3D ( 'NONE', #17761, #8942, #19765 ) ;
#18545 = VECTOR ( 'NONE', #14083, 1000.000000000000000 ) ;
#18546 = CARTESIAN_POINT ( 'NONE',  ( -8.216162181246543739, -12.44282262938666328, 7.299847320220930413 ) ) ;
#18547 = VECTOR ( 'NONE', #10122, 1000.000000000000000 ) ;
#18548 = CARTESIAN_POINT ( 'NONE',  ( -7.026577802269633466, -2.648906230146649943, 8.453373545151602997 ) ) ;
#18549 = DIRECTION ( 'NONE',  ( 7.860214984770699307E-18, -1.409037165336591006E-16, -1.000000000000000000 ) ) ;
#18550 = DIRECTION ( 'NONE',  ( 0.000000000000000000, 0.000000000000000000, 1.000000000000000000 ) ) ;
#18551 = CARTESIAN_POINT ( 'NONE',  ( -4.578118944855224193, 1.701165921963350813, -1.570465384416952936 ) ) ;
#18552 = DIRECTION ( 'NONE',  ( -4.190823558986626092E-31, 1.000000000000000000, 4.190823558986610327E-31 ) ) ;
#18553 = DIRECTION ( 'NONE',  ( -1.000000000000000000, -4.440892098500626162E-16, 5.551115123125782702E-16 ) ) ;
#18554 = VERTEX_POINT ( 'NONE', #10705 ) ;
#18555 = B_SPLINE_CURVE_WITH_KNOTS ( 'NONE', 3,
 ( #15865, #21543, #7075, #19647, #3309, #5064 ),
 .UNSPECIFIED., .F., .F.,
 ( 4, 2, 4 ),
 ( 0.002365888236227973399, 0.003551327329835062430, 0.004736766423442151895 ),
 .UNSPECIFIED. ) ;
#18556 = EDGE_CURVE ( 'NONE', #9771, #3527, #8678, .T. ) ;
#18557 = CIRCLE ( 'NONE', #8427, 2.550000000000003819 ) ;
#18558 = VERTEX_POINT ( 'NONE', #1538 ) ;
#18559 = CIRCLE ( 'NONE', #19315, 2.550000000000010481 ) ;
#18560 = EDGE_LOOP ( 'NONE', ( #9064, #14597 ) ) ;
#18561 = AXIS2_PLACEMENT_3D ( 'NONE', #1246, #21478, #23246 ) ;
#18562 = ADVANCED_FACE ( 'NONE', ( #8711 ), #15867, .T. ) ;
#18563 = CARTESIAN_POINT ( 'NONE',  ( 119.5756419024615269, -4.500000000000003553, 6.500000000000123457 ) ) ;
#18564 = EDGE_LOOP ( 'NONE', ( #7569, #16152, #19544, #11485 ) ) ;
#18565 =( REPRESENTATION_RELATIONSHIP ('NONE','NONE', #19450, #11650 ) REPRESENTATION_RELATIONSHIP_WITH_TRANSFORMATION ( #9643 )SHAPE_REPRESENTATION_RELATIONSHIP( ) );
#18566 = CARTESIAN_POINT ( 'NONE',  ( 0.2499999999999932832, 1.250000000000042633, -2.000000000000001776 ) ) ;
#18567 = CARTESIAN_POINT ( 'NONE',  ( 2.499999999999981348, 4.250000000000087041, -17.50000000000001776 ) ) ;
#18568 = PLANE ( 'NONE',  #12469 ) ;
#18569 = ORIENTED_EDGE ( 'NONE', *, *, #11871, .T. ) ;
#18570 = EDGE_CURVE ( 'NONE', #17901, #20601, #20239, .T. ) ;
#18571 = FACE_OUTER_BOUND ( 'NONE', #14972, .T. ) ;
#18572 = CARTESIAN_POINT ( 'NONE',  ( 0.000000000000000000, 0.000000000000000000, 0.000000000000000000 ) ) ;
#18573 = ADVANCED_FACE ( 'NONE', ( #9523 ), #2230, .F. ) ;
#18574 = ORIENTED_EDGE ( 'NONE', *, *, #6079, .T. ) ;
#18575 = PLANE ( 'NONE',  #22226 ) ;
#18576 = EDGE_CURVE ( 'NONE', #6390, #15040, #4103, .T. ) ;
#18577 = CARTESIAN_POINT ( 'NONE',  ( 7.473326079327807570, -13.84852298796451997, 7.598194856234284700 ) ) ;
#18578 = CARTESIAN_POINT ( 'NONE',  ( 7.991520206789753722, -13.39565235458638881, 7.599114430427904132 ) ) ;
#18579 = TOROIDAL_SURFACE ( 'NONE', #1304, 2.500000000000002220, 0.5000000000000000000 ) ;
#18580 = FACE_OUTER_BOUND ( 'NONE', #8268, .T. ) ;
#18581 = CONICAL_SURFACE ( 'NONE', #19654, 4.000000000000000000, 1.047197551196595855 ) ;
#18582 = CYLINDRICAL_SURFACE ( 'NONE', #16641, 0.5000000000000028866 ) ;
#18583 = LINE ( 'NONE', #13174, #21743 ) ;
#18584 = COLOUR_RGB ( '', 0.09019608, 0.27058824, 0.51372549) ;
#18585 = CARTESIAN_POINT ( 'NONE',  ( 37.50000000000012790, -1.677151478558897161E-14, -2.316987298107702209 ) ) ;
#18586 = CARTESIAN_POINT ( 'NONE',  ( 3.878096787214415642, -3.381939201670079775, -1.142309474598505181 ) ) ;
#18587 = ORIENTED_EDGE ( 'NONE', *, *, #7419, .F. ) ;
#18588 = ADVANCED_FACE ( 'NONE', ( #14584 ), #22111, .T. ) ;
#18589 = ADVANCED_FACE ( 'NONE', ( #9635 ), #18236, .T. ) ;
#18590 = ORIENTED_EDGE ( 'NONE', *, *, #11099, .F. ) ;
#18591 = CIRCLE ( 'NONE', #9953, 2.500000000000015987 ) ;
#18593 = ORIENTED_EDGE ( 'NONE', *, *, #8232, .T. ) ;
#18592 = ORIENTED_EDGE ( 'NONE', *, *, #22639, .F. ) ;
#18594 = CIRCLE ( 'NONE', #8459, 0.5000000000000029976 ) ;
#18595 = EDGE_CURVE ( 'NONE', #23027, #7941, #1308, .T. ) ;
#18596 = CARTESIAN_POINT ( 'NONE',  ( -6.999999999999992006, -5.999999999999987566, 6.250000000000005329 ) ) ;
#18597 = CARTESIAN_POINT ( 'NONE',  ( 0.6666666666666055674, -4.233901974057364015, -3.300726591567105572 ) ) ;
#18598 = DIRECTION ( 'NONE',  ( -1.000000000000000000, 1.550910762415526064E-16, 0.000000000000000000 ) ) ;
#18599 = ADVANCED_FACE ( 'NONE', ( #709 ), #23054, .F. ) ;
#18600 = CARTESIAN_POINT ( 'NONE',  ( -3.674234614174765046, -0.7499999999999451550, -3.000000000000051070 ) ) ;
#18601 = CARTESIAN_POINT ( 'NONE',  ( -50.65685424949277404, -0.5000000000000905942, -7.500000000000062172 ) ) ;
#18602 = ADVANCED_FACE ( 'NONE', ( #20345 ), #18582, .T. ) ;
#18603 = CARTESIAN_POINT ( 'NONE',  ( -67.28510754798011817, -2.700000000000125855, 12.22107821754960000 ) ) ;
#18604 = CARTESIAN_POINT ( 'NONE',  ( -6.525612274168518745, 36.03379296756838812, -17.36249956737804112 ) ) ;
#18605 = FILL_AREA_STYLE_COLOUR ( '', #20078 ) ;
#18606 = DIRECTION ( 'NONE',  ( 6.656013887802287108E-31, 1.000000000000000000, -3.469446951953609061E-15 ) ) ;
#18607 = CARTESIAN_POINT ( 'NONE',  ( 2.775557561562891351E-14, 0.5000000000000004441, -6.499999999999950262 ) ) ;
#18608 =( NAMED_UNIT ( * ) PLANE_ANGLE_UNIT ( ) SI_UNIT ( $, .RADIAN. ) );
#18609 = CIRCLE ( 'NONE', #12442, 3.499999999999999556 ) ;
#18610 = DIRECTION ( 'NONE',  ( 0.000000000000000000, 0.000000000000000000, -1.000000000000000000 ) ) ;
#18611 = CARTESIAN_POINT ( 'NONE',  ( 0.4500000002918510544, 42.99999999900385461, -19.49999999999998934 ) ) ;
#18612 = DIRECTION ( 'NONE',  ( 1.000000000000000000, -4.190823558986610327E-31, 1.733449886265890494E-32 ) ) ;
#18613 = CARTESIAN_POINT ( 'NONE',  ( -55.05572809000123868, -1.040834085586084257E-13, -7.500000000000062172 ) ) ;
#18614 = ORIENTED_EDGE ( 'NONE', *, *, #6786, .T. ) ;
#18615 =( LENGTH_UNIT ( ) NAMED_UNIT ( * ) SI_UNIT ( .MILLI., .METRE. ) );
#18617 = ORIENTED_EDGE ( 'NONE', *, *, #5410, .F. ) ;
#18616 = ORIENTED_EDGE ( 'NONE', *, *, #10131, .T. ) ;
#18618 = ORIENTED_EDGE ( 'NONE', *, *, #1770, .T. ) ;
#18620 = ORIENTED_EDGE ( 'NONE', *, *, #22056, .F. ) ;
#18619 = EDGE_LOOP ( 'NONE', ( #21525, #2346, #9949, #10571 ) ) ;
#18621 = EDGE_LOOP ( 'NONE', ( #7481, #16714 ) ) ;
#18622 = EDGE_CURVE ( 'NONE', #14963, #6361, #17012, .T. ) ;
#18623 = CARTESIAN_POINT ( 'NONE',  ( 119.5756419024615269, -4.000000000000003553, 6.500000000000123457 ) ) ;
#18624 = DIRECTION ( 'NONE',  ( 5.551115123125677932E-17, 0.000000000000000000, -1.000000000000000000 ) ) ;
#18625 = ORIENTED_EDGE ( 'NONE', *, *, #17222, .F. ) ;
#18626 = CARTESIAN_POINT ( 'NONE',  ( 0.2175679805369863662, -1.691499766289382256, -3.500000000000010214 ) ) ;
#18627 = DIRECTION ( 'NONE',  ( 1.000000000000000000, 0.000000000000000000, 0.000000000000000000 ) ) ;
#18628 = DIRECTION ( 'NONE',  ( -1.000000000000000000, -2.220446049250311109E-15, 0.000000000000000000 ) ) ;
#18629 = FACE_OUTER_BOUND ( 'NONE', #12029, .T. ) ;
#18630 = DIRECTION ( 'NONE',  ( 0.000000000000000000, 0.000000000000000000, 1.000000000000000000 ) ) ;
#18631 = CARTESIAN_POINT ( 'NONE',  ( 2.000000000000015543, -3.464101615137746837, -5.600000000000000533 ) ) ;
#18632 = DIRECTION ( 'NONE',  ( 5.551115123125782702E-16, 1.201780285297635172E-31, -1.000000000000000000 ) ) ;
#18633 = CARTESIAN_POINT ( 'NONE',  ( -7.499999999999992895, -5.999999999999987566, 6.249999999999992006 ) ) ;
#18634 = CARTESIAN_POINT ( 'NONE',  ( -4.690415759824456465, -0.7499999999999242828, -1.999999999999849010 ) ) ;
#18635 = CARTESIAN_POINT ( 'NONE',  ( -7.000000000000006217, -6.999999999999995559, 10.75000000000000888 ) ) ;
#18636 = DIRECTION ( 'NONE',  ( 1.000000000000000000, 1.734723475976796001E-16, 0.000000000000000000 ) ) ;
#18637 = DIRECTION ( 'NONE',  ( 1.333893503340774882E-15, 2.778352770573747380E-17, 1.000000000000000000 ) ) ;
#18638 = VERTEX_POINT ( 'NONE', #4327 ) ;
#18639 = SURFACE_STYLE_FILL_AREA ( #20413 ) ;
#18641 = VERTEX_POINT ( 'NONE', #16560 ) ;
#18640 = VERTEX_POINT ( 'NONE', #11392 ) ;
#18642 = ORIENTED_EDGE ( 'NONE', *, *, #22120, .F. ) ;
#18643 = VECTOR ( 'NONE', #18225, 1000.000000000000000 ) ;
#18644 = VERTEX_POINT ( 'NONE', #467 ) ;
#18645 = VERTEX_POINT ( 'NONE', #16680 ) ;
#18646 = ADVANCED_FACE ( 'NONE', ( #2457 ), #21110, .F. ) ;
#18647 = CIRCLE ( 'NONE', #1010, 2.550000000000002043 ) ;
#18648 = EDGE_LOOP ( 'NONE', ( #14429, #9101, #11544, #1531 ) ) ;
#18649 = CARTESIAN_POINT ( 'NONE',  ( 4.082498951862915781, -2.020725942163708488, 3.500000000000004885 ) ) ;
#18650 = CARTESIAN_POINT ( 'NONE',  ( 0.2499999999999516498, 0.2500000000000140998, -2.000000000000001776 ) ) ;
#18651 = VERTEX_POINT ( 'NONE', #7530 ) ;
#18652 = EDGE_CURVE ( 'NONE', #5077, #7485, #21878, .T. ) ;
#18653 = CARTESIAN_POINT ( 'NONE',  ( -42.54314575050795355, 3.999999999999996447, -7.500000000000007105 ) ) ;
#18654 = FACE_OUTER_BOUND ( 'NONE', #19814, .T. ) ;
#18655 = DIRECTION ( 'NONE',  ( -0.7313537016191731244, 0.6819983600624957010, -5.924440990721420203E-17 ) ) ;
#18656 = CARTESIAN_POINT ( 'NONE',  ( 31.55000000029185259, 16.99999999900385461, -15.99999999999999289 ) ) ;
#18657 = CARTESIAN_POINT ( 'NONE',  ( -8.954763739086862628, -14.00000000000004441, 6.678571428571461688 ) ) ;
#18658 = DIRECTION ( 'NONE',  ( 0.000000000000000000, 0.000000000000000000, 1.000000000000000000 ) ) ;
#18659 = CARTESIAN_POINT ( 'NONE',  ( -6.999999999708142795, 13.99999999900385106, -19.00000000000000355 ) ) ;
#18660 = CARTESIAN_POINT ( 'NONE',  ( -3.200000000000036149, -2.000000000000043521, 8.000000000000047962 ) ) ;
#18661 = AXIS2_PLACEMENT_3D ( 'NONE', #19337, #1453, #19446 ) ;
#18662 = EDGE_CURVE ( 'NONE', #11952, #4887, #8227, .T. ) ;
#18663 =( NAMED_UNIT ( * ) PLANE_ANGLE_UNIT ( ) SI_UNIT ( $, .RADIAN. ) );
#18664 = DIRECTION ( 'NONE',  ( 2.013525853228518840E-32, -6.902532920683810383E-31, 1.000000000000000000 ) ) ;
#18665 = CARTESIAN_POINT ( 'NONE',  ( 2.775557561562891351E-14, 0.000000000000000000, -3.000000000000002665 ) ) ;
#18667 = ORIENTED_EDGE ( 'NONE', *, *, #6081, .F. ) ;
#18666 = AXIS2_PLACEMENT_3D ( 'NONE', #1344, #19560, #19687 ) ;
#18668 = ORIENTED_EDGE ( 'NONE', *, *, #4641, .T. ) ;
#18669 = VERTEX_POINT ( 'NONE', #6692 ) ;
#18670 = ORIENTED_EDGE ( 'NONE', *, *, #4036, .F. ) ;
#18671 = ORIENTED_EDGE ( 'NONE', *, *, #4454, .T. ) ;
#18672 = CARTESIAN_POINT ( 'NONE',  ( -4.000000000000003553, 0.3904826640788073289, -5.599999999999998757 ) ) ;
#18673 = EDGE_LOOP ( 'NONE', ( #11547, #11436, #3637 ) ) ;
#18674 = B_SPLINE_CURVE_WITH_KNOTS ( 'NONE', 3,
 ( #1213, #6615, #22508, #10369, #13562, #20744 ),
 .UNSPECIFIED., .F., .F.,
 ( 4, 2, 4 ),
 ( 0.006456566858647396628, 0.007625406818786647362, 0.008794246778925898095 ),
 .UNSPECIFIED. ) ;
#18675 = CARTESIAN_POINT ( 'NONE',  ( 6.500000000000227374, 1.665334536937734811E-13, 6.000000000000213163 ) ) ;
#18676 = CARTESIAN_POINT ( 'NONE',  ( 30.00000000029184832, -9.961476088449217059E-10, -39.00000000000000000 ) ) ;
#18677 = CIRCLE ( 'NONE', #659, 0.2500000000000000000 ) ;
#18678 = DIRECTION ( 'NONE',  ( -1.000000000000000000, 0.000000000000000000, -4.336808689941968432E-16 ) ) ;
#18679 = DIRECTION ( 'NONE',  ( 4.190823558986625216E-31, -1.000000000000000000, 4.190823558986625216E-31 ) ) ;
#18680 = DIRECTION ( 'NONE',  ( -0.000000000000000000, -0.000000000000000000, 1.000000000000000000 ) ) ;
#18681 = CARTESIAN_POINT ( 'NONE',  ( 4.484160662959468802, 0.7500000000000558442, -2.618649729759251699 ) ) ;
#18682 = CARTESIAN_POINT ( 'NONE',  ( 0.000000000000000000, 0.000000000000000000, 0.000000000000000000 ) ) ;
#18683 = PRODUCT_RELATED_PRODUCT_CATEGORY ( 'part', '', ( #12303 ) ) ;
#18684 = DIRECTION ( 'NONE',  ( 1.000000000000000000, -4.440892098500650814E-16, -7.860214984771115307E-18 ) ) ;
#18685 = CIRCLE ( 'NONE', #682, 2.000000000000000000 ) ;
#18686 = CARTESIAN_POINT ( 'NONE',  ( -50.65685424949267457, -7.200000000000071232, -8.000000000000007105 ) ) ;
#18687 = CARTESIAN_POINT ( 'NONE',  ( 3.878096787214418750, 2.680238624821010163, -2.357690525401503923 ) ) ;
#18688 = PLANE ( 'NONE',  #14595 ) ;
#18690 = CIRCLE ( 'NONE', #14929, 3.749999999999989786 ) ;
#18689 = CARTESIAN_POINT ( 'NONE',  ( 1.312671235360332256, 3.860931062424256321, -0.05923475698271866291 ) ) ;
#18691 = EDGE_CURVE ( 'NONE', #774, #11851, #11751, .T. ) ;
#18692 = DIRECTION ( 'NONE',  ( 0.4999999999999997780, 5.044886816051349048E-16, 0.8660254037844387076 ) ) ;
#18693 = CIRCLE ( 'NONE', #6314, 0.4999999999999995559 ) ;
#18694 = ORIENTED_EDGE ( 'NONE', *, *, #3735, .T. ) ;
#18695 = VECTOR ( 'NONE', #16588, 1000.000000000000000 ) ;
#18696 = EDGE_CURVE ( 'NONE', #3791, #12006, #8091, .T. ) ;
#18697 = CONTEXT_DEPENDENT_SHAPE_REPRESENTATION ( #5804, #16062 ) ;
#18698 = ORIENTED_EDGE ( 'NONE', *, *, #18361, .F. ) ;
#18699 = APPLICATION_CONTEXT ( 'automotive_design' ) ;
#18700 = EDGE_CURVE ( 'NONE', #22681, #14484, #6460, .T. ) ;
#18701 = CIRCLE ( 'NONE', #1814, 4.500000000000045297 ) ;
#18703 = ORIENTED_EDGE ( 'NONE', *, *, #15785, .F. ) ;
#18702 = ORIENTED_EDGE ( 'NONE', *, *, #12459, .F. ) ;
#18704 = LINE ( 'NONE', #11875, #18547 ) ;
#18705 = AXIS2_PLACEMENT_3D ( 'NONE', #10384, #8743, #6995 ) ;
#18706 = DIRECTION ( 'NONE',  ( 1.733449886265891589E-32, -4.190823558986610327E-31, 1.000000000000000000 ) ) ;
#18707 = DIRECTION ( 'NONE',  ( -0.8660254037844378194, -0.5000000000000014433, -1.169077423688995342E-15 ) ) ;
#18708 = CARTESIAN_POINT ( 'NONE',  ( 6.999999999999992006, -8.000000000000051514, 6.249999999999977796 ) ) ;
#18709 = DIRECTION ( 'NONE',  ( 0.000000000000000000, 0.000000000000000000, 1.000000000000000000 ) ) ;
#18710 = CARTESIAN_POINT ( 'NONE',  ( -89.70000000000059970, 2.700000000000056577, 1.000000000000000888 ) ) ;
#18711 = PRESENTATION_LAYER_ASSIGNMENT (  '', '', ( #2189 ) ) ;
#18713 = EDGE_CURVE ( 'NONE', #15682, #11574, #16258, .T. ) ;
#18712 = DIRECTION ( 'NONE',  ( 0.000000000000000000, 0.000000000000000000, -1.000000000000000000 ) ) ;
#18714 = DIRECTION ( 'NONE',  ( 0.7313537016191731244, -0.6819983600624958120, 5.924440990721420203E-17 ) ) ;
#18715 = CARTESIAN_POINT ( 'NONE',  ( -0.3263565795980838957, 4.430380094434251959, -0.2484800633750068877 ) ) ;
#18716 =( NAMED_UNIT ( * ) SI_UNIT ( $, .STERADIAN. ) SOLID_ANGLE_UNIT ( ) );
#18717 = ADVANCED_FACE ( 'NONE', ( #19048 ), #9994, .T. ) ;
#18718 = AXIS2_PLACEMENT_3D ( 'NONE', #7507, #20094, #569 ) ;
#18719 = CARTESIAN_POINT ( 'NONE',  ( 0.3126073911696447549, 4.041451884327362798, -2.081668171172168513E-14 ) ) ;
#18720 = CIRCLE ( 'NONE', #17203, 3.499999999999996003 ) ;
#18721 = DIRECTION ( 'NONE',  ( 1.000000000000000000, -1.389842848855773367E-62, 2.013525853228507892E-32 ) ) ;
#18722 = AXIS2_PLACEMENT_3D ( 'NONE', #11101, #14751, #7814 ) ;
#18723 = CARTESIAN_POINT ( 'NONE',  ( 42.00000000000017764, 2.999999999999999112, 2.000000000000057288 ) ) ;
#18724 = DIRECTION ( 'NONE',  ( 2.172745813409349776E-17, -1.000000000000000000, 1.309377075419428048E-16 ) ) ;
#18725 = ORIENTED_EDGE ( 'NONE', *, *, #7234, .F. ) ;
#18726 = EDGE_CURVE ( 'NONE', #12296, #4090, #6896, .T. ) ;
#18727 =( NAMED_UNIT ( * ) PLANE_ANGLE_UNIT ( ) SI_UNIT ( $, .RADIAN. ) );
#18728 = ADVANCED_FACE ( 'NONE', ( #1289 ), #18812, .F. ) ;
#18730 = ORIENTED_EDGE ( 'NONE', *, *, #6708, .T. ) ;
#18729 = ORIENTED_EDGE ( 'NONE', *, *, #9824, .F. ) ;
#18731 = ORIENTED_EDGE ( 'NONE', *, *, #21101, .F. ) ;
#18732 = ORIENTED_EDGE ( 'NONE', *, *, #18766, .F. ) ;
#18734 = ORIENTED_EDGE ( 'NONE', *, *, #18823, .F. ) ;
#18733 = VERTEX_POINT ( 'NONE', #22461 ) ;
#18735 = ORIENTED_EDGE ( 'NONE', *, *, #11706, .T. ) ;
#18736 = CARTESIAN_POINT ( 'NONE',  ( 6.000000000291855429, -0.5000000009961480529, -39.00000000000000000 ) ) ;
#18737 = FACE_OUTER_BOUND ( 'NONE', #18619, .T. ) ;
#18738 = ORIENTED_EDGE ( 'NONE', *, *, #13892, .F. ) ;
#18739 = FILL_AREA_STYLE ('',( #9576 ) ) ;
#18740 = AXIS2_PLACEMENT_3D ( 'NONE', #5514, #12676, #5039 ) ;
#18741 = VECTOR ( 'NONE', #3015, 1000.000000000000000 ) ;
#18742 = DIRECTION ( 'NONE',  ( -2.220446049250313081E-16, 1.000000000000000000, -7.025792437124636392E-31 ) ) ;
#18743 = DIRECTION ( 'NONE',  ( 0.000000000000000000, -1.000000000000000000, 0.000000000000000000 ) ) ;
#18744 = LINE ( 'NONE', #6170, #13544 ) ;
#18745 = EDGE_CURVE ( 'NONE', #20539, #20452, #8336, .T. ) ;
#18746 = CARTESIAN_POINT ( 'NONE',  ( -95.70000000000058549, -2.700000000000119194, 1.000000000000014655 ) ) ;
#18747 = EDGE_CURVE ( 'NONE', #11343, #5312, #2817, .T. ) ;
#18748 = EDGE_CURVE ( 'NONE', #10144, #17843, #21563, .T. ) ;
#18749 = PLANE ( 'NONE',  #3876 ) ;
#18750 = CARTESIAN_POINT ( 'NONE',  ( 7.638377885296685932, -1.936221580214098292, 8.340398698103570041 ) ) ;
#18751 = DIRECTION ( 'NONE',  ( 1.454462294001240516E-30, 1.000000000000000000, 0.000000000000000000 ) ) ;
#18752 = DIRECTION ( 'NONE',  ( -1.000000000000000000, 1.550910762415510534E-16, 0.000000000000000000 ) ) ;
#18753 =( GEOMETRIC_REPRESENTATION_CONTEXT ( 3 ) GLOBAL_UNCERTAINTY_ASSIGNED_CONTEXT ( ( #15214 ) ) GLOBAL_UNIT_ASSIGNED_CONTEXT ( ( #12260, #17680, #10511 ) ) REPRESENTATION_CONTEXT ( 'NONE', 'WORKASPACE' ) );
#18754 = CARTESIAN_POINT ( 'NONE',  ( 0.000000000000000000, 1.750000000000001554, 0.000000000000000000 ) ) ;
#18755 = CARTESIAN_POINT ( 'NONE',  ( -64.00000000000045475, 2.700000000000056577, -1.999999999999974021 ) ) ;
#18756 = CARTESIAN_POINT ( 'NONE',  ( -6.999999999708142795, 13.99999999900385106, -26.00000000000000000 ) ) ;
#18757 = ADVANCED_FACE ( 'NONE', ( #15385 ), #13865, .T. ) ;
#18758 = FACE_OUTER_BOUND ( 'NONE', #10972, .T. ) ;
#18759 = EDGE_LOOP ( 'NONE', ( #15072, #2851 ) ) ;
#18760 = UNCERTAINTY_MEASURE_WITH_UNIT (LENGTH_MEASURE( 1.000000000000000082E-05 ), #20735, 'distance_accuracy_value', 'NONE');
#18761 = AXIS2_PLACEMENT_3D ( 'NONE', #7479, #16511, #4162 ) ;
#18762 = EDGE_CURVE ( 'NONE', #4432, #14457, #7269, .T. ) ;
#18763 = TOROIDAL_SURFACE ( 'NONE', #2597, 4.500000000000000888, 0.5000000000000000000 ) ;
#18765 = VERTEX_POINT ( 'NONE', #11972 ) ;
#18764 = EDGE_LOOP ( 'NONE', ( #3973, #17743 ) ) ;
#18766 = EDGE_CURVE ( 'NONE', #14732, #273, #8106, .T. ) ;
#18767 = ORIENTED_EDGE ( 'NONE', *, *, #4501, .T. ) ;
#18768 = ORIENTED_EDGE ( 'NONE', *, *, #8112, .T. ) ;
#18769 = VECTOR ( 'NONE', #8475, 1000.000000000000114 ) ;
#18770 = ORIENTED_EDGE ( 'NONE', *, *, #18311, .F. ) ;
#18771 = PRODUCT_DEFINITION_FORMATION_WITH_SPECIFIED_SOURCE ( 'ANY', '', #4976, .NOT_KNOWN. ) ;
#18772 = ORIENTED_EDGE ( 'NONE', *, *, #11815, .F. ) ;
#18773 = CARTESIAN_POINT ( 'NONE',  ( 4.071447262713884463, 4.041451884327383226, 0.000000000000000000 ) ) ;
#18774 = CARTESIAN_POINT ( 'NONE',  ( 30.60000000000000142, 2.775557561562891351E-14, 2.054999999999978844 ) ) ;
#18775 = ORIENTED_EDGE ( 'NONE', *, *, #7690, .F. ) ;
#18776 = DIRECTION ( 'NONE',  ( -1.000000000000000000, -5.598259082250514647E-17, -3.330669073875432643E-16 ) ) ;
#18777 = CARTESIAN_POINT ( 'NONE',  ( 4.151274195509681242, 2.039912954708690052, 3.533232880573531798 ) ) ;
#18778 = DIRECTION ( 'NONE',  ( -0.7071067811865232589, 0.7071067811865717756, 0.000000000000000000 ) ) ;
#18779 = DIRECTION ( 'NONE',  ( 0.000000000000000000, 0.000000000000000000, 1.000000000000000000 ) ) ;
#18780 = DIRECTION ( 'NONE',  ( 3.032184104443272185E-30, 1.000000000000000000, -7.395570986447005381E-32 ) ) ;
#18781 = CARTESIAN_POINT ( 'NONE',  ( 3.000000000000002665, 0.000000000000000000, 0.000000000000000000 ) ) ;
#18782 = VECTOR ( 'NONE', #17076, 1000.000000000000114 ) ;
#18783 = CARTESIAN_POINT ( 'NONE',  ( 2.918498775983380256E-10, 6.999999999003851947, -29.00000000000000355 ) ) ;
#18784 = EDGE_CURVE ( 'NONE', #4468, #8523, #18160, .T. ) ;
#18785 = CARTESIAN_POINT ( 'NONE',  ( -6.463109109390148576E-15, -22.91099746826335348, 10.34816708862275547 ) ) ;
#18786 = ORIENTED_EDGE ( 'NONE', *, *, #14672, .T. ) ;
#18787 = SURFACE_SIDE_STYLE ('',( #8080 ) ) ;
#18788 = DIRECTION ( 'NONE',  ( 1.000000000000000000, 1.479114197289397135E-31, 5.916456789157588541E-31 ) ) ;
#18789 = B_SPLINE_CURVE_WITH_KNOTS ( 'NONE', 3,
 ( #13835, #15814, #1594, #15935 ),
 .UNSPECIFIED., .F., .F.,
 ( 4, 4 ),
 ( 2.380735702073125514E-07, 0.002775112046897006829 ),
 .UNSPECIFIED. ) ;
#18790 = DIRECTION ( 'NONE',  ( 0.6819983600625072473, 0.7313537016191623552, 0.000000000000000000 ) ) ;
#18791 = ORIENTED_EDGE ( 'NONE', *, *, #16304, .F. ) ;
#18792 = ADVANCED_FACE ( 'NONE', ( #4909, #10208 ), #20701, .T. ) ;
#18793 = B_SPLINE_CURVE_WITH_KNOTS ( 'NONE', 3,
 ( #21939, #3586, #10866, #5829, #3923, #11217 ),
 .UNSPECIFIED., .F., .F.,
 ( 4, 2, 4 ),
 ( 0.006456566858647415710, 0.007625406818786682923, 0.008794246778925950137 ),
 .UNSPECIFIED. ) ;
#18794 = ORIENTED_EDGE ( 'NONE', *, *, #8498, .T. ) ;
#18795 = ORIENTED_EDGE ( 'NONE', *, *, #13244, .T. ) ;
#18796 = ORIENTED_EDGE ( 'NONE', *, *, #18766, .T. ) ;
#18797 = ORIENTED_EDGE ( 'NONE', *, *, #7960, .T. ) ;
#18798 = CARTESIAN_POINT ( 'NONE',  ( 3.951447005078448260, 2.357513599190970144, 2.916666666666664742 ) ) ;
#18799 = FACE_OUTER_BOUND ( 'NONE', #17327, .T. ) ;
#18800 = ORIENTED_EDGE ( 'NONE', *, *, #11939, .T. ) ;
#18801 = CIRCLE ( 'NONE', #13561, 0.4999999999999994449 ) ;
#18802 = CYLINDRICAL_SURFACE ( 'NONE', #12091, 2.500000000000003553 ) ;
#18803 = CARTESIAN_POINT ( 'NONE',  ( 12.49999999999995914, 2.775557561562891036E-14, -4.500000000000002665 ) ) ;
#18804 = DIRECTION ( 'NONE',  ( 2.013525853228507892E-32, 6.902532920683810383E-31, -1.000000000000000000 ) ) ;
#18805 = EDGE_CURVE ( 'NONE', #3237, #8906, #17792, .T. ) ;
#18806 = CARTESIAN_POINT ( 'NONE',  ( -4.993857080238742974, 35.99999999900384751, -19.46409504053740491 ) ) ;
#18807 = CARTESIAN_POINT ( 'NONE',  ( -95.20000000000065654, 2.700000000000014833, 8.000000000000076383 ) ) ;
#18808 = DIRECTION ( 'NONE',  ( 4.190823558986626092E-31, -1.000000000000000000, -4.190823558986610327E-31 ) ) ;
#18809 = CYLINDRICAL_SURFACE ( 'NONE', #3157, 6.249999999999992006 ) ;
#18810 = DIRECTION ( 'NONE',  ( 0.000000000000000000, -1.000000000000000000, 0.000000000000000000 ) ) ;
#18811 = DIRECTION ( 'NONE',  ( 1.000000000000000000, 4.264528545109623427E-14, 0.000000000000000000 ) ) ;
#18812 = PLANE ( 'NONE',  #1274 ) ;
#18813 = CARTESIAN_POINT ( 'NONE',  ( -12.84999999999999964, -0.5000000000000038858, 6.250000000000033751 ) ) ;
#18814 = LINE ( 'NONE', #3513, #11121 ) ;
#18815 = LINE ( 'NONE', #13757, #2179 ) ;
#18816 = AXIS2_PLACEMENT_3D ( 'NONE', #12218, #19405, #15863 ) ;
#18817 = ORIENTED_EDGE ( 'NONE', *, *, #12988, .T. ) ;
#18818 = ORIENTED_EDGE ( 'NONE', *, *, #8272, .F. ) ;
#18820 = EDGE_LOOP ( 'NONE', ( #7540, #9851, #3861, #6034 ) ) ;
#18819 = ORIENTED_EDGE ( 'NONE', *, *, #14126, .T. ) ;
#18821 = CARTESIAN_POINT ( 'NONE',  ( 33.94974746859769255, 21.94974746730969528, -29.00000000000000355 ) ) ;
#18822 = DIRECTION ( 'NONE',  ( 0.000000000000000000, 6.802837160693368935E-15, 1.000000000000000000 ) ) ;
#18823 = EDGE_CURVE ( 'NONE', #16867, #4929, #7166, .T. ) ;
#18824 = SURFACE_STYLE_USAGE ( .BOTH. , #14942 ) ;
#18825 = EDGE_LOOP ( 'NONE', ( #9096, #2178, #18625, #3847 ) ) ;
#18826 = AXIS2_PLACEMENT_3D ( 'NONE', #12521, #1480, #8540 ) ;
#18827 = DIRECTION ( 'NONE',  ( -1.000000000000000000, -3.254448077276381206E-32, -1.066788928082016908E-26 ) ) ;
#18828 = CARTESIAN_POINT ( 'NONE',  ( -4.000000000000003553, 2.309401076758494487, -5.600000000000000533 ) ) ;
#18829 = CARTESIAN_POINT ( 'NONE',  ( -3.200000000000091660, 1.999999999999980904, -8.000000000000035527 ) ) ;
#18830 = CARTESIAN_POINT ( 'NONE',  ( 12.49999999999995914, 2.775557561562891351E-14, -9.500000000000003553 ) ) ;
#18831 = CARTESIAN_POINT ( 'NONE',  ( 5.100000000000007638, 0.000000000000000000, 0.000000000000000000 ) ) ;
#18832 = DIRECTION ( 'NONE',  ( 1.000000000000000000, -2.168404344971005170E-16, 1.203141491611682442E-30 ) ) ;
#18833 = CARTESIAN_POINT ( 'NONE',  ( -2.000000000000015543, 3.464101615137746837, -5.600000000000000533 ) ) ;
#18834 = DIRECTION ( 'NONE',  ( 1.000000000000000000, -1.550910762415513985E-16, -3.012982189080959477E-32 ) ) ;
#18835 = CARTESIAN_POINT ( 'NONE',  ( -6.000000000000088818, -2.000000000000043521, -7.500000000000007105 ) ) ;
#18836 = DIRECTION ( 'NONE',  ( 2.891205793294678326E-16, 1.000000000000000000, 0.000000000000000000 ) ) ;
#18837 = LINE ( 'NONE', #2843, #5580 ) ;
#18838 = CARTESIAN_POINT ( 'NONE',  ( -6.000000000000074607, -5.300000000000027356, -7.500000000000034639 ) ) ;
#18839 = ORIENTED_EDGE ( 'NONE', *, *, #10404, .T. ) ;
#18840 = TOROIDAL_SURFACE ( 'NONE', #18107, 6.500000000000000888, 0.5000000000000000000 ) ;
#18842 = EDGE_LOOP ( 'NONE', ( #15197, #9066, #16634, #7655 ) ) ;
#18841 = EDGE_LOOP ( 'NONE', ( #808, #7057 ) ) ;
#18843 = VERTEX_POINT ( 'NONE', #19383 ) ;
#18844 = EDGE_CURVE ( 'NONE', #23235, #7692, #20412, .T. ) ;
#18846 = ORIENTED_EDGE ( 'NONE', *, *, #5954, .T. ) ;
#18845 = ORIENTED_EDGE ( 'NONE', *, *, #12669, .T. ) ;
#18847 = LINE ( 'NONE', #4496, #18529 ) ;
#18848 = DIRECTION ( 'NONE',  ( -1.550910762415566494E-16, -1.000000000000000000, 8.135128085091684243E-31 ) ) ;
#18849 = EDGE_CURVE ( 'NONE', #22937, #9917, #105, .T. ) ;
#18850 = ORIENTED_EDGE ( 'NONE', *, *, #15065, .F. ) ;
#18851 = SURFACE_SIDE_STYLE ('',( #13212 ) ) ;
#18852 = FACE_OUTER_BOUND ( 'NONE', #22794, .T. ) ;
#18853 = DIRECTION ( 'NONE',  ( 1.000000000000000000, 2.699383410053119644E-30, 3.330669073875432643E-16 ) ) ;
#18854 = CARTESIAN_POINT ( 'NONE',  ( 22.49999999999993960, 4.250000000000045297, -17.75000000000001066 ) ) ;
#18855 = CARTESIAN_POINT ( 'NONE',  ( 2.918498775983380256E-10, -9.961476088449217059E-10, -39.00000000000000000 ) ) ;
#18856 = EDGE_CURVE ( 'NONE', #15286, #12036, #1625, .T. ) ;
#18857 = DIRECTION ( 'NONE',  ( 0.5150787536377134934, 0.000000000000000000, -0.8571428571428567622 ) ) ;
#18858 = DIRECTION ( 'NONE',  ( -1.939787525279694947E-32, 6.902532920683810383E-31, -1.000000000000000000 ) ) ;
#18859 = CIRCLE ( 'NONE', #21871, 7.000000000000075495 ) ;
#18860 = AXIS2_PLACEMENT_3D ( 'NONE', #8095, #15255, #4094 ) ;
#18861 = EDGE_CURVE ( 'NONE', #5698, #20776, #5773, .T. ) ;
#18862 = CARTESIAN_POINT ( 'NONE',  ( 3.972058292797657320, 0.6948821373597494633, 3.565770528409099249 ) ) ;
#18863 = DIRECTION ( 'NONE',  ( -1.858632295689435609E-16, -1.000000000000000000, 0.000000000000000000 ) ) ;
#18864 = EDGE_CURVE ( 'NONE', #11435, #2970, #14219, .T. ) ;
#18865 = PRESENTATION_LAYER_ASSIGNMENT (  '', '', ( #1640 ) ) ;
#18866 = DIRECTION ( 'NONE',  ( -1.000000000000000000, -2.220446049250301001E-16, 0.000000000000000000 ) ) ;
#18867 = CARTESIAN_POINT ( 'NONE',  ( -55.05572809000126711, 3.200000000000022382, -7.500000000000034639 ) ) ;
#18868 = CARTESIAN_POINT ( 'NONE',  ( 2.060000000000013820, -2.630118345336998747E-15, -0.3080913168122645374 ) ) ;
#18869 = CARTESIAN_POINT ( 'NONE',  ( -47.47487373415330580, 4.018019484660594109, -8.000000000000062172 ) ) ;
#18870 = PRODUCT ( 'Link', 'Link', '', ( #11055 ) ) ;
#18871 = VERTEX_POINT ( 'NONE', #8686 ) ;
#18872 = CONICAL_SURFACE ( 'NONE', #22248, 2.500000000000002220, 0.9599310885968830309 ) ;
#18874 = ORIENTED_EDGE ( 'NONE', *, *, #8096, .F. ) ;
#18873 = ORIENTED_EDGE ( 'NONE', *, *, #3128, .F. ) ;
#18875 = EDGE_CURVE ( 'NONE', #22258, #21644, #3137, .T. ) ;
#18876 =( BOUNDED_SURFACE ( )  B_SPLINE_SURFACE ( 3, 2, ( 
 ( #8809, #1515, #3628 ),
 ( #15737, #22934, #23169 ),
 ( #6932, #14097, #21521 ),
 ( #106, #7051, #5158 ),
 ( #14221, #8688, #7284 ),
 ( #14326, #1850, #23268 ) ),
 .UNSPECIFIED., .F., .F., .T. ) 
 B_SPLINE_SURFACE_WITH_KNOTS ( ( 4, 2, 4 ),
 ( 3, 3 ),
 ( 0.02032853247518125878, 0.02278863295364821559, 0.02524873343211517240 ),
 ( 0.000000000000000000, 1.000000000000000000 ),
 .UNSPECIFIED. ) 
 GEOMETRIC_REPRESENTATION_ITEM ( )  RATIONAL_B_SPLINE_SURFACE ( (
 ( 1.000000000000000000, 0.8047781615896834051, 1.000000000000000000),
 ( 1.000000000000000000, 0.8123767586290329135, 1.000000000000000000),
 ( 1.000000000000000000, 0.8190662415562958154, 1.000000000000000000),
 ( 1.000000000000000000, 0.8192361015670447388, 1.000000000000000000),
 ( 1.000000000000000000, 0.8126135807102816688, 1.000000000000000000),
 ( 1.000000000000000000, 0.8047712338318578906, 1.000000000000000000) ) ) 
 REPRESENTATION_ITEM ( '' )  SURFACE ( )  );
#18877 = ORIENTED_EDGE ( 'NONE', *, *, #20460, .T. ) ;
#18878 = EDGE_CURVE ( 'NONE', #17901, #21212, #19507, .T. ) ;
#18879 = ADVANCED_FACE ( 'NONE', ( #8920, #19265 ), #3402, .F. ) ;
#18880 = EDGE_LOOP ( 'NONE', ( #18738, #15544, #378, #13228 ) ) ;
#18881 = AXIS2_PLACEMENT_3D ( 'NONE', #10870, #16385, #14296 ) ;
#18882 = CIRCLE ( 'NONE', #478, 0.5000000000000004441 ) ;
#18883 = AXIS2_PLACEMENT_3D ( 'NONE', #3832, #18207, #2073 ) ;
#18884 = CIRCLE ( 'NONE', #21144, 5.749999999999992006 ) ;
#18885 = ORIENTED_EDGE ( 'NONE', *, *, #22769, .F. ) ;
#18886 = CARTESIAN_POINT ( 'NONE',  ( -50.65685424949270299, 7.200000000000025935, 7.500000000000062172 ) ) ;
#18887 = CARTESIAN_POINT ( 'NONE',  ( 10.50000000000000888, -2.000000000000001776, 5.750000000000005329 ) ) ;
#18888 = VERTEX_POINT ( 'NONE', #17737 ) ;
#18889 = ADVANCED_FACE ( 'NONE', ( #17499 ), #7644, .T. ) ;
#18890 = ORIENTED_EDGE ( 'NONE', *, *, #21313, .T. ) ;
#18891 = DIRECTION ( 'NONE',  ( -1.000000000000000000, -2.699383410053119644E-30, -3.330669073875432643E-16 ) ) ;
#18892 = CARTESIAN_POINT ( 'NONE',  ( 2.742413778650823364, 1.325747111984056037, -4.750000000000000888 ) ) ;
#18893 = EDGE_CURVE ( 'NONE', #12775, #11851, #21172, .T. ) ;
#18894 = DIRECTION ( 'NONE',  ( 1.733449886265891589E-32, -4.190823558986610327E-31, 1.000000000000000000 ) ) ;
#18895 = DIRECTION ( 'NONE',  ( 1.000000000000000000, 0.000000000000000000, 0.000000000000000000 ) ) ;
#18896 = CARTESIAN_POINT ( 'NONE',  ( 5.484827557301452217, -1.325747111984059590, 0.000000000000000000 ) ) ;
#18897 = CARTESIAN_POINT ( 'NONE',  ( -7.161440864725725497, -11.61224748569070364, 7.973376427817314038 ) ) ;
#18898 = EDGE_CURVE ( 'NONE', #8787, #6638, #8773, .T. ) ;
#18899 = DIRECTION ( 'NONE',  ( 1.000000000000000000, -4.440892098500655744E-16, 7.860214984770760936E-18 ) ) ;
#18900 = PLANE ( 'NONE',  #20636 ) ;
#18901 = AXIS2_PLACEMENT_3D ( 'NONE', #19790, #3442, #21225 ) ;
#18902 = DIRECTION ( 'NONE',  ( 1.000000000000000000, 2.168404344971017743E-16, -1.780660105995169760E-30 ) ) ;
#18903 = AXIS2_PLACEMENT_3D ( 'NONE', #7698, #9002, #5473 ) ;
#18904 = CARTESIAN_POINT ( 'NONE',  ( 27.94974746859769255, 27.94974746730969528, -18.50000000000000355 ) ) ;
#18905 = AXIS2_PLACEMENT_3D ( 'NONE', #17080, #4739, #11907 ) ;
#18906 = EDGE_LOOP ( 'NONE', ( #13202, #1305, #15631, #17714 ) ) ;
#18907 = AXIS2_PLACEMENT_3D ( 'NONE', #14938, #20485, #18365 ) ;
#18908 = SURFACE_STYLE_USAGE ( .BOTH. , #18787 ) ;
#18909 = FACE_OUTER_BOUND ( 'NONE', #18974, .T. ) ;
#18910 = CARTESIAN_POINT ( 'NONE',  ( 2.499999999999988454, 4.500000000000059508, -1.250000000000028866 ) ) ;
#18911 = VERTEX_POINT ( 'NONE', #15842 ) ;
#18912 = ORIENTED_EDGE ( 'NONE', *, *, #15823, .T. ) ;
#18913 = ORIENTED_EDGE ( 'NONE', *, *, #19750, .F. ) ;
#18914 = VERTEX_POINT ( 'NONE', #19747 ) ;
#18915 = FACE_OUTER_BOUND ( 'NONE', #11341, .T. ) ;
#18916 = CARTESIAN_POINT ( 'NONE',  ( -89.70000000000054285, -0.5000000000000628386, 1.000000000000000888 ) ) ;
#18917 = AXIS2_PLACEMENT_3D ( 'NONE', #12558, #1735, #21408 ) ;
#18918 = ORIENTED_EDGE ( 'NONE', *, *, #16914, .F. ) ;
#18919 = TOROIDAL_SURFACE ( 'NONE', #19673, 5.500000000000000000, 0.5000000000000000000 ) ;
#18920 = CARTESIAN_POINT ( 'NONE',  ( 2.775557561562891351E-14, 7.999999999999983125, 2.500000000000057732 ) ) ;
#18921 = CIRCLE ( 'NONE', #8416, 7.000000000000075495 ) ;
#18922 = EDGE_CURVE ( 'NONE', #16805, #7255, #14777, .T. ) ;
#18923 = PLANE ( 'NONE',  #21314 ) ;
#18924 = DIRECTION ( 'NONE',  ( 2.168404344970994323E-16, -1.000000000000000000, 1.577721810442023611E-30 ) ) ;
#18925 = TOROIDAL_SURFACE ( 'NONE', #13667, 2.500000000000000000, 0.5000000000000000000 ) ;
#18926 = CARTESIAN_POINT ( 'NONE',  ( -6.231825765915511184, 35.99999999900384751, -18.98541138272435802 ) ) ;
#18927 = CARTESIAN_POINT ( 'NONE',  ( 4.033901012036328559, 2.321269032827576684, 2.979444097106367817 ) ) ;
#18928 = CARTESIAN_POINT ( 'NONE',  ( -50.65685424949281668, 2.700000000000021938, -7.500000000000089706 ) ) ;
#18929 = EDGE_CURVE ( 'NONE', #14402, #13088, #17983, .T. ) ;
#18930 = CARTESIAN_POINT ( 'NONE',  ( 2.775557561562891351E-14, 10.75000000000000000, -6.499999999999950262 ) ) ;
#18931 = CARTESIAN_POINT ( 'NONE',  ( 0.000000000000000000, 0.000000000000000000, 0.000000000000000000 ) ) ;
#18932 = FACE_OUTER_BOUND ( 'NONE', #9304, .T. ) ;
#18933 = CARTESIAN_POINT ( 'NONE',  ( -6.938893903907228378E-14, 4.999999999999976907, -4.163336342344337027E-14 ) ) ;
#18934 = DIRECTION ( 'NONE',  ( -0.7071067811865457964, 0.7071067811865492381, 0.000000000000000000 ) ) ;
#18935 = LINE ( 'NONE', #22463, #7376 ) ;
#18936 = CIRCLE ( 'NONE', #151, 6.000000000000000000 ) ;
#18937 = CARTESIAN_POINT ( 'NONE',  ( -2.171643655288394648, 3.365003104552311441, 2.155275334288567213E-15 ) ) ;
#18938 = VECTOR ( 'NONE', #16739, 1000.000000000000000 ) ;
#18939 = VERTEX_POINT ( 'NONE', #3168 ) ;
#18940 = TOROIDAL_SURFACE ( 'NONE', #2389, 6.500000000000000888, 0.5000000000000000000 ) ;
#18941 = ITEM_DEFINED_TRANSFORMATION ( 'NONE', 'NONE', #19523,  #22115 ) ;
#18942 = VERTEX_POINT ( 'NONE', #10330 ) ;
#18944 = ORIENTED_EDGE ( 'NONE', *, *, #21250, .T. ) ;
#18943 = ORIENTED_EDGE ( 'NONE', *, *, #8855, .T. ) ;
#18945 = CARTESIAN_POINT ( 'NONE',  ( 82.19834661797897013, -4.499999999999809930, 6.500000000000151879 ) ) ;
#18946 = DIRECTION ( 'NONE',  ( 1.000000000000000000, 0.000000000000000000, 0.000000000000000000 ) ) ;
#18947 = FACE_OUTER_BOUND ( 'NONE', #19274, .T. ) ;
#18948 = VECTOR ( 'NONE', #4508, 1000.000000000000000 ) ;
#18949 = EDGE_LOOP ( 'NONE', ( #17092, #17628, #15545, #2555 ) ) ;
#18950 = CIRCLE ( 'NONE', #21548, 2.550000000000002043 ) ;
#18951 = CARTESIAN_POINT ( 'NONE',  ( 3.191783008269905686, -1.561572887838375889, 3.971669662941499368 ) ) ;
#18952 = CARTESIAN_POINT ( 'NONE',  ( -52.60445557845680753, -0.5000000000000281997, 15.85914177512520773 ) ) ;
#18953 = CIRCLE ( 'NONE', #23098, 6.500000000000075495 ) ;
#18954 = EDGE_CURVE ( 'NONE', #16755, #6059, #1395, .T. ) ;
#18955 = CARTESIAN_POINT ( 'NONE',  ( 42.50000000000020606, 2.999999999999999112, -13.00000000000002487 ) ) ;
#18956 = CARTESIAN_POINT ( 'NONE',  ( -1.040834085586084257E-13, 4.862606272033151100, -3.745885042887441063 ) ) ;
#18957 = CARTESIAN_POINT ( 'NONE',  ( -3.499999999708153453, 13.99999999900385106, -26.00000000000000000 ) ) ;
#18958 = CARTESIAN_POINT ( 'NONE',  ( 0.2174200650117315003, 3.876582599186173095, 0.2855619784720343501 ) ) ;
#18959 = DIRECTION ( 'NONE',  ( -7.860214984771176937E-18, -1.409037165336591006E-16, -1.000000000000000000 ) ) ;
#18960 = DIRECTION ( 'NONE',  ( -1.000000000000000000, 4.190823558986610327E-31, -1.733449886265890494E-32 ) ) ;
#18961 = FACE_OUTER_BOUND ( 'NONE', #3463, .T. ) ;
#18962 = DIRECTION ( 'NONE',  ( 1.000000000000000000, 2.220446049250314067E-16, -5.825996348268307008E-33 ) ) ;
#18963 = DIRECTION ( 'NONE',  ( -2.220446049250313081E-16, 1.000000000000000000, -7.025792437124636392E-31 ) ) ;
#18964 = ORIENTED_EDGE ( 'NONE', *, *, #12081, .F. ) ;
#18965 = EDGE_CURVE ( 'NONE', #17392, #21322, #809, .T. ) ;
#18966 = TOROIDAL_SURFACE ( 'NONE', #11445, 5.200000000000001066, 0.4999999999999978351 ) ;
#18967 = DIRECTION ( 'NONE',  ( 1.000000000000000000, 0.000000000000000000, 0.000000000000000000 ) ) ;
#18968 = CIRCLE ( 'NONE', #21977, 3.500000000000004441 ) ;
#18970 = EDGE_LOOP ( 'NONE', ( #19307, #3820, #9673, #6537 ) ) ;
#18969 = EDGE_LOOP ( 'NONE', ( #13210, #8238 ) ) ;
#18971 = UNCERTAINTY_MEASURE_WITH_UNIT (LENGTH_MEASURE( 1.000000000000000082E-05 ), #16343, 'distance_accuracy_value', 'NONE');
#18972 = ORIENTED_EDGE ( 'NONE', *, *, #9821, .F. ) ;
#18974 = EDGE_LOOP ( 'NONE', ( #22031, #20943, #21832, #8750, #22953, #13598, #15715 ) ) ;
#18973 = ORIENTED_EDGE ( 'NONE', *, *, #4507, .F. ) ;
#18975 = ORIENTED_EDGE ( 'NONE', *, *, #6196, .T. ) ;
#18976 = DIRECTION ( 'NONE',  ( -1.733449886265890494E-32, 7.264582621685754939E-63, 1.000000000000000000 ) ) ;
#18977 = DIRECTION ( 'NONE',  ( 0.000000000000000000, 3.469446951953616555E-15, 1.000000000000000000 ) ) ;
#18978 = CARTESIAN_POINT ( 'NONE',  ( 113.0166151911346759, -11.64708151429785765, -6.500000000000040856 ) ) ;
#18979 =( BOUNDED_CURVE ( )  B_SPLINE_CURVE ( 3, ( #9465, #20644, #4512, #11677 ),
 .UNSPECIFIED., .F., .F. ) 
 B_SPLINE_CURVE_WITH_KNOTS ( ( 4, 4 ),
 ( 1.570796326794896558, 2.617993877991540597 ),
 .UNSPECIFIED. ) 
 CURVE ( )  GEOMETRIC_REPRESENTATION_ITEM ( )  RATIONAL_B_SPLINE_CURVE ( ( 1.000000000000000000, 0.9106836025229513298, 0.9106836025229513298, 1.000000000000000000 ) ) 
 REPRESENTATION_ITEM ( '' )  );
#18980 = CARTESIAN_POINT ( 'NONE',  ( -50.65685424949274562, -1.040834085586084257E-13, 8.000000000000062172 ) ) ;
#18981 = DIRECTION ( 'NONE',  ( -2.775557561562883647E-17, 3.406761633869147840E-16, -1.000000000000000000 ) ) ;
#18982 = CARTESIAN_POINT ( 'NONE',  ( 2.498001805406602216E-16, -1.291058893185205491E-15, -4.499999999999988454 ) ) ;
#18983 = AXIS2_PLACEMENT_3D ( 'NONE', #17619, #21516, #8803 ) ;
#18984 = CYLINDRICAL_SURFACE ( 'NONE', #13306, 0.5000000000000004441 ) ;
#18985 = CARTESIAN_POINT ( 'NONE',  ( 4.204115023516959759, -1.660442669500223012, -3.602151381774619132 ) ) ;
#18986 = MECHANICAL_DESIGN_GEOMETRIC_PRESENTATION_REPRESENTATION (  '', ( #23127 ), #11095 ) ;
#18987 = DIRECTION ( 'NONE',  ( -3.330669073875432643E-16, -4.437342591868153746E-31, 1.000000000000000000 ) ) ;
#18988 = DIRECTION ( 'NONE',  ( -0.6819983600624976994, -0.7313537016191713480, 0.000000000000000000 ) ) ;
#18989 = CARTESIAN_POINT ( 'NONE',  ( -7.000000000000020428, -8.000000000000010658, 10.74999999999998224 ) ) ;
#18990 = CARTESIAN_POINT ( 'NONE',  ( -4.000000000000002665, -0.7779732554280794909, -0.03354435108168014879 ) ) ;
#18991 = CARTESIAN_POINT ( 'NONE',  ( -8.715898959466873208, -12.49756837761075978, 6.833978265954060660 ) ) ;
#18992 = LINE ( 'NONE', #11683, #15316 ) ;
#18993 = CYLINDRICAL_SURFACE ( 'NONE', #10400, 0.5000000000000000000 ) ;
#18994 = ORIENTED_EDGE ( 'NONE', *, *, #22390, .F. ) ;
#18995 = EDGE_CURVE ( 'NONE', #16118, #8988, #6525, .T. ) ;
#18997 = ORIENTED_EDGE ( 'NONE', *, *, #9645, .T. ) ;
#18996 = ORIENTED_EDGE ( 'NONE', *, *, #22779, .T. ) ;
#18998 = B_SPLINE_CURVE_WITH_KNOTS ( 'NONE', 3,
 ( #18221, #13035, #13157, #7623, #21860, #1858, #4191, #12920, #2087, #17993, #9043, #16434, #16540, #340, #20099, #3971, #20219, #11148, #16199, #14461 ),
 .UNSPECIFIED., .F., .F.,
 ( 4, 2, 2, 2, 2, 2, 2, 2, 2, 4 ),
 ( 0.0005000078514897923158, 0.001232179299099181967, 0.001964350746708571835, 0.002696522194317961703, 0.003062607918122655336, 0.003428693641927348969, 0.004160865089536750980, 0.004893036537146153858, 0.005625207984755555869, 0.006357379432364958748 ),
 .UNSPECIFIED. ) ;
#18999 = ORIENTED_EDGE ( 'NONE', *, *, #18311, .T. ) ;
#19000 = EDGE_CURVE ( 'NONE', #12774, #21109, #2430, .T. ) ;
#19001 = VERTEX_POINT ( 'NONE', #10898 ) ;
#19002 = CONICAL_SURFACE ( 'NONE', #14108, 4.750000000000000000, 1.047197551196600074 ) ;
#19003 = EDGE_LOOP ( 'NONE', ( #13903, #12922 ) ) ;
#19004 = EDGE_CURVE ( 'NONE', #13876, #19780, #9612, .T. ) ;
#19005 = ORIENTED_EDGE ( 'NONE', *, *, #3392, .T. ) ;
#19006 = DIRECTION ( 'NONE',  ( -0.9878135252003127365, 1.532010627492774434E-16, 0.1556420233463029767 ) ) ;
#19007 = AXIS2_PLACEMENT_3D ( 'NONE', #153, #16011, #7890 ) ;
#19008 = DIRECTION ( 'NONE',  ( 1.000000000000000000, 0.000000000000000000, 1.613696256722611405E-16 ) ) ;
#19009 = EDGE_LOOP ( 'NONE', ( #5285, #22603, #15064, #1384 ) ) ;
#19010 = EDGE_LOOP ( 'NONE', ( #2002, #11956 ) ) ;
#19011 = DIRECTION ( 'NONE',  ( -1.000000000000000000, -4.252453317207022018E-31, 5.551115123125818447E-17 ) ) ;
#19012 = CARTESIAN_POINT ( 'NONE',  ( 0.000000000000000000, 1.387778780781445676E-14, -25.03750572909315508 ) ) ;
#19013 = CARTESIAN_POINT ( 'NONE',  ( 4.124214193018063135, 2.028338413290941666, 3.513185186763571721 ) ) ;
#19014 = FACE_OUTER_BOUND ( 'NONE', #516, .T. ) ;
#19015 = CARTESIAN_POINT ( 'NONE',  ( -91.02295700146262902, 2.700000000000014833, 6.338518968055040226 ) ) ;
#19016 = FACE_BOUND ( 'NONE', #13061, .T. ) ;
#19017 = ADVANCED_FACE ( 'NONE', ( #18091 ), #15012, .T. ) ;
#19018 = CARTESIAN_POINT ( 'NONE',  ( -4.000000000000095923, 0.1981133338132648469, -6.980680862638442631E-14 ) ) ;
#19019 = EDGE_CURVE ( 'NONE', #6944, #10401, #11396, .T. ) ;
#19020 = DIRECTION ( 'NONE',  ( -2.220446049250313081E-16, 1.000000000000000000, -7.025792437124636392E-31 ) ) ;
#19021 = CARTESIAN_POINT ( 'NONE',  ( 0.1388410611046085874, 3.710337782248036120, 0.5735064479039790886 ) ) ;
#19022 = CARTESIAN_POINT ( 'NONE',  ( 37.46001462128849369, 0.1698019261547604186, -10.46001462128817927 ) ) ;
#19023 = ORIENTED_EDGE ( 'NONE', *, *, #2640, .F. ) ;
#19024 = ADVANCED_FACE ( 'NONE', ( #7729 ), #7288, .T. ) ;
#19025 =( NAMED_UNIT ( * ) SI_UNIT ( $, .STERADIAN. ) SOLID_ANGLE_UNIT ( ) );
#19026 = CARTESIAN_POINT ( 'NONE',  ( 27.94974746859769255, 27.94974746730969528, -29.00000000000000355 ) ) ;
#19027 = ORIENTED_EDGE ( 'NONE', *, *, #3989, .T. ) ;
#19028 = VECTOR ( 'NONE', #18322, 1000.000000000000000 ) ;
#19029 = EDGE_CURVE ( 'NONE', #4343, #19925, #17403, .T. ) ;
#19030 = ORIENTED_EDGE ( 'NONE', *, *, #10810, .F. ) ;
#19031 = ORIENTED_EDGE ( 'NONE', *, *, #9598, .T. ) ;
#19032 = ORIENTED_EDGE ( 'NONE', *, *, #12401, .F. ) ;
#19033 = DIRECTION ( 'NONE',  ( -1.000000000000000000, 1.492474417944849379E-16, 3.760416335592108037E-33 ) ) ;
#19034 = CARTESIAN_POINT ( 'NONE',  ( 2.775557561562891351E-14, 0.000000000000000000, -6.499999999999950262 ) ) ;
#19035 = ORIENTED_EDGE ( 'NONE', *, *, #18209, .T. ) ;
#19036 = CARTESIAN_POINT ( 'NONE',  ( -3.414274948570314550, -9.020562075079396891E-14, -21.66938530120587814 ) ) ;
#19037 = DIRECTION ( 'NONE',  ( 1.000000000000000000, 5.501551595240671658E-14, 3.717264591378832268E-16 ) ) ;
#19038 = CARTESIAN_POINT ( 'NONE',  ( 0.2174200650117711076, -2.185595227304893307, 3.214438021527944667 ) ) ;
#19039 = CIRCLE ( 'NONE', #14149, 0.4999999999999984457 ) ;
#19040 = DIRECTION ( 'NONE',  ( 0.000000000000000000, 0.000000000000000000, 1.000000000000000000 ) ) ;
#19041 = CARTESIAN_POINT ( 'NONE',  ( -3.414274948570314550, -0.5000000000000768274, -21.66938530120587814 ) ) ;
#19042 = EDGE_CURVE ( 'NONE', #12423, #9711, #7502, .T. ) ;
#19043 = EDGE_CURVE ( 'NONE', #12774, #22329, #7387, .T. ) ;
#19044 = VECTOR ( 'NONE', #16968, 1000.000000000000000 ) ;
#19045 = DIRECTION ( 'NONE',  ( -1.000000000000000000, -3.254448077276381206E-32, -1.066788928082016908E-26 ) ) ;
#19046 = EDGE_CURVE ( 'NONE', #1035, #10173, #9265, .T. ) ;
#19047 = CARTESIAN_POINT ( 'NONE',  ( 2.775557561562891351E-14, 2.499999999999995115, -12.50000000000001066 ) ) ;
#19048 = FACE_OUTER_BOUND ( 'NONE', #20450, .T. ) ;
#19049 = LINE ( 'NONE', #21282, #14178 ) ;
#19050 = DIRECTION ( 'NONE',  ( -1.000000000000000000, -2.699383410053119644E-30, -3.330669073875432643E-16 ) ) ;
#19051 = ORIENTED_EDGE ( 'NONE', *, *, #17691, .T. ) ;
#19052 = EDGE_CURVE ( 'NONE', #21109, #16622, #2202, .T. ) ;
#19053 = ORIENTED_EDGE ( 'NONE', *, *, #16403, .T. ) ;
#19054 = CIRCLE ( 'NONE', #11906, 9.500000000000056843 ) ;
#19056 = ORIENTED_EDGE ( 'NONE', *, *, #6635, .T. ) ;
#19055 = ORIENTED_EDGE ( 'NONE', *, *, #16274, .T. ) ;
#19057 = DIRECTION ( 'NONE',  ( 1.000000000000000000, 2.699383410053119644E-30, 3.330669073875432643E-16 ) ) ;
#19058 = FACE_OUTER_BOUND ( 'NONE', #7201, .T. ) ;
#19059 = CARTESIAN_POINT ( 'NONE',  ( 2.742413778650823364, -1.325747111984059590, -4.750000000000000888 ) ) ;
#19060 = VECTOR ( 'NONE', #14325, 1000.000000000000000 ) ;
#19061 = ORIENTED_EDGE ( 'NONE', *, *, #18112, .T. ) ;
#19062 = CARTESIAN_POINT ( 'NONE',  ( 26.45000000029184051, 16.99999999900385461, -15.99999999999999289 ) ) ;
#19063 = DIRECTION ( 'NONE',  ( -0.000000000000000000, 1.000000000000000000, 0.000000000000000000 ) ) ;
#19064 = PRODUCT_DEFINITION_SHAPE ( 'NONE', 'NONE',  #2001 ) ;
#19065 = DIRECTION ( 'NONE',  ( -1.000000000000000000, 0.000000000000000000, 0.000000000000000000 ) ) ;
#19066 = CARTESIAN_POINT ( 'NONE',  ( -42.54314575050795355, 3.999999999999996447, -7.500000000000007105 ) ) ;
#19067 = TOROIDAL_SURFACE ( 'NONE', #22838, 2.500000000000000000, 0.5000000000000000000 ) ;
#19068 = LINE ( 'NONE', #11885, #17048 ) ;
#19069 = DIRECTION ( 'NONE',  ( 0.7071067811865435759, -3.270568595685441704E-16, -0.7071067811865514585 ) ) ;
#19070 = DIRECTION ( 'NONE',  ( -1.333893503340774882E-15, -2.778352770573747380E-17, -1.000000000000000000 ) ) ;
#19071 = AXIS2_PLACEMENT_3D ( 'NONE', #16426, #21751, #5632 ) ;
#19072 = CARTESIAN_POINT ( 'NONE',  ( -55.25320565519140104, -3.200000000000108979, 7.500000000000047962 ) ) ;
#19073 = AXIS2_PLACEMENT_3D ( 'NONE', #12696, #10700, #21654 ) ;
#19074 = EDGE_CURVE ( 'NONE', #4924, #7803, #9915, .T. ) ;
#19075 = ORIENTED_EDGE ( 'NONE', *, *, #19935, .T. ) ;
#19076 = AXIS2_PLACEMENT_3D ( 'NONE', #2372, #6261, #18721 ) ;
#19078 = ORIENTED_EDGE ( 'NONE', *, *, #16080, .T. ) ;
#19077 = VERTEX_POINT ( 'NONE', #5741 ) ;
#19079 = VECTOR ( 'NONE', #20988, 1000.000000000000000 ) ;
#19080 = ADVANCED_FACE ( 'NONE', ( #12912 ), #20090, .F. ) ;
#19081 = ORIENTED_EDGE ( 'NONE', *, *, #10671, .F. ) ;
#19083 = ORIENTED_EDGE ( 'NONE', *, *, #15415, .F. ) ;
#19082 = EDGE_LOOP ( 'NONE', ( #15794, #19576, #3880, #20050 ) ) ;
#19084 = DIRECTION ( 'NONE',  ( -0.000000000000000000, -0.000000000000000000, 1.000000000000000000 ) ) ;
#19085 = AXIS2_PLACEMENT_3D ( 'NONE', #19802, #10853, #14617 ) ;
#19086 = CARTESIAN_POINT ( 'NONE',  ( 6.000000000291855429, 2.999999999003851503, -8.549999999999998934 ) ) ;
#19087 = DIRECTION ( 'NONE',  ( 0.000000000000000000, 0.000000000000000000, 1.000000000000000000 ) ) ;
#19088 = LINE ( 'NONE', #2979, #21652 ) ;
#19089 = DIRECTION ( 'NONE',  ( -3.885780586188016830E-16, -4.437342591868156373E-31, 1.000000000000000000 ) ) ;
#19090 = CARTESIAN_POINT ( 'NONE',  ( -7.972478112619597823, -1.636497393431879610, 7.628219499134209158 ) ) ;
#19091 = VECTOR ( 'NONE', #18239, 1000.000000000000000 ) ;
#19092 = FACE_OUTER_BOUND ( 'NONE', #7004, .T. ) ;
#19093 = CARTESIAN_POINT ( 'NONE',  ( 4.000000000000349054, 0.8228435280415953290, -3.430609588141484423 ) ) ;
#19094 = VECTOR ( 'NONE', #17289, 1000.000000000000000 ) ;
#19095 = DIRECTION ( 'NONE',  ( -1.000000000000000000, -6.224605580259554159E-31, 2.887593071917436153E-31 ) ) ;
#19096 = AXIS2_PLACEMENT_3D ( 'NONE', #4656, #6549, #19119 ) ;
#19097 = CARTESIAN_POINT ( 'NONE',  ( 4.180345472528530948, 2.086001522971435485, 3.570468649087180424 ) ) ;
#19098 = CARTESIAN_POINT ( 'NONE',  ( 37.00000000000014211, 11.00000000000000000, -3.000000000000002665 ) ) ;
#19099 = DIRECTION ( 'NONE',  ( 0.000000000000000000, -1.000000000000000000, 0.000000000000000000 ) ) ;
#19100 = DIRECTION ( 'NONE',  ( -0.000000000000000000, -0.000000000000000000, 1.000000000000000000 ) ) ;
#19101 = DIRECTION ( 'NONE',  ( 1.454462294001240516E-30, 1.000000000000000000, 0.000000000000000000 ) ) ;
#19102 = CARTESIAN_POINT ( 'NONE',  ( -50.65685424949281668, 0.5000000000000143219, 7.500000000000034639 ) ) ;
#19103 = VERTEX_POINT ( 'NONE', #13027 ) ;
#19105 = VERTEX_POINT ( 'NONE', #20320 ) ;
#19104 = ORIENTED_EDGE ( 'NONE', *, *, #488, .T. ) ;
#19106 = VERTEX_POINT ( 'NONE', #2310 ) ;
#19107 = AXIS2_PLACEMENT_3D ( 'NONE', #14453, #15846, #12202 ) ;
#19108 = ORIENTED_EDGE ( 'NONE', *, *, #55, .T. ) ;
#19109 = TOROIDAL_SURFACE ( 'NONE', #20617, 2.250000000000000444, 0.2500000000000000000 ) ;
#19110 = ORIENTED_EDGE ( 'NONE', *, *, #22146, .F. ) ;
#19111 = ORIENTED_EDGE ( 'NONE', *, *, #11532, .F. ) ;
#19112 = CARTESIAN_POINT ( 'NONE',  ( 3.000000000291852764, 42.99999999900385461, -18.50000000000000355 ) ) ;
#19113 = CARTESIAN_POINT ( 'NONE',  ( 0.2175679805409919676, -1.691499766303336649, 3.499999999999960032 ) ) ;
#19114 = ORIENTED_EDGE ( 'NONE', *, *, #19042, .F. ) ;
#19115 = DIRECTION ( 'NONE',  ( -1.000000000000000000, 0.000000000000000000, 0.000000000000000000 ) ) ;
#19116 = DIRECTION ( 'NONE',  ( 1.733449886265890494E-32, 4.190823558986611203E-31, -1.000000000000000000 ) ) ;
#19117 = EDGE_CURVE ( 'NONE', #6327, #8147, #16653, .T. ) ;
#19118 = FACE_OUTER_BOUND ( 'NONE', #2503, .T. ) ;
#19119 = DIRECTION ( 'NONE',  ( -1.000000000000000000, 6.938893903907186568E-15, 0.000000000000000000 ) ) ;
#19120 = DIRECTION ( 'NONE',  ( 2.220446049250313081E-16, -1.000000000000000000, 7.025792437124636392E-31 ) ) ;
#19121 = FACE_OUTER_BOUND ( 'NONE', #22916, .T. ) ;
#19122 = CARTESIAN_POINT ( 'NONE',  ( -8.510464245293324126, -13.49280278100719421, 6.988717072694019095 ) ) ;
#19123 = AXIS2_PLACEMENT_3D ( 'NONE', #18032, #14147, #21226 ) ;
#19124 = LINE ( 'NONE', #22663, #18741 ) ;
#19125 = AXIS2_PLACEMENT_3D ( 'NONE', #15591, #22781, #6656 ) ;
#19126 = AXIS2_PLACEMENT_3D ( 'NONE', #2424, #9259, #2537 ) ;
#19127 = DIRECTION ( 'NONE',  ( 0.000000000000000000, -1.000000000000000000, 0.000000000000000000 ) ) ;
#19128 = DIRECTION ( 'NONE',  ( -1.000000000000000000, -2.699383410053119644E-30, -3.330669073875432643E-16 ) ) ;
#19129 = EDGE_LOOP ( 'NONE', ( #15308, #949, #4837, #3692 ) ) ;
#19130 = CARTESIAN_POINT ( 'NONE',  ( 3.973110223768751226, -0.6864646529411689846, -3.565797985667510606 ) ) ;
#19131 = FACE_OUTER_BOUND ( 'NONE', #12619, .T. ) ;
#19132 = CIRCLE ( 'NONE', #12392, 1.300000000000009592 ) ;
#19133 = ORIENTED_EDGE ( 'NONE', *, *, #2620, .F. ) ;
#19134 = ADVANCED_FACE ( 'NONE', ( #22083 ), #19294, .T. ) ;
#19135 = COLOUR_RGB ( '', 0.08235294, 0.09019608, 0.10196078) ;
#19136 = VERTEX_POINT ( 'NONE', #18783 ) ;
#19137 = ORIENTED_EDGE ( 'NONE', *, *, #23210, .T. ) ;
#19138 = EDGE_LOOP ( 'NONE', ( #17352, #5821, #17069, #8663, #22614 ) ) ;
#19139 = CARTESIAN_POINT ( 'NONE',  ( 5.036205380386656216, 1.584759246591015414, -0.7770364038185831879 ) ) ;
#19140 = EDGE_CURVE ( 'NONE', #18130, #11317, #17032, .T. ) ;
#19141 = DIRECTION ( 'NONE',  ( -1.000000000000000000, 1.424116703980815236E-16, 2.931272055834072749E-32 ) ) ;
#19142 = ORIENTED_EDGE ( 'NONE', *, *, #2958, .F. ) ;
#19143 = CARTESIAN_POINT ( 'NONE',  ( -12.85000000000001386, -1.499999999999997780, -5.749999999999976907 ) ) ;
#19144 = DIRECTION ( 'NONE',  ( 0.1556420233463076119, 0.000000000000000000, 0.9878135252003121813 ) ) ;
#19145 = DIRECTION ( 'NONE',  ( 1.000000000000000000, 0.000000000000000000, 0.000000000000000000 ) ) ;
#19146 = EDGE_CURVE ( 'NONE', #84, #4283, #16994, .T. ) ;
#19147 = CARTESIAN_POINT ( 'NONE',  ( -4.775149780314047909, 35.99999999900384751, -19.49999996803511237 ) ) ;
#19148 = CARTESIAN_POINT ( 'NONE',  ( 4.180231891692593571, 2.049421325483134826, 3.591231015387239545 ) ) ;
#19149 = AXIS2_PLACEMENT_3D ( 'NONE', #4762, #11931, #18891 ) ;
#19150 = APPLICATION_CONTEXT ( 'automotive_design' ) ;
#19151 = CARTESIAN_POINT ( 'NONE',  ( -7.500000000000020428, -1.390227771353544473, 9.250000000000014211 ) ) ;
#19152 = PRODUCT_DEFINITION_FORMATION_WITH_SPECIFIED_SOURCE ( 'ANY', '', #17360, .NOT_KNOWN. ) ;
#19153 = CARTESIAN_POINT ( 'NONE',  ( 0.000000000000000000, -0.5999999999999859890, 3.054668707061614086 ) ) ;
#19154 = CARTESIAN_POINT ( 'NONE',  ( 7.499999999999978684, -8.000000000000051514, 6.249999999999977796 ) ) ;
#19155 = EDGE_CURVE ( 'NONE', #12162, #5230, #13986, .T. ) ;
#19156 = EDGE_CURVE ( 'NONE', #19457, #11731, #13254, .T. ) ;
#19157 = CARTESIAN_POINT ( 'NONE',  ( 77.42435809754135789, -6.499999999999811706, 6.500000000000137668 ) ) ;
#19158 = DIRECTION ( 'NONE',  ( -1.000000000000000000, 0.000000000000000000, -3.330669073875427220E-16 ) ) ;
#19160 = EDGE_CURVE ( 'NONE', #6752, #14012, #18936, .T. ) ;
#19159 = FACE_BOUND ( 'NONE', #17900, .T. ) ;
#19161 = CARTESIAN_POINT ( 'NONE',  ( 2.742413778650823364, 1.749999999999998002, -4.750000000000024869 ) ) ;
#19162 = ORIENTED_EDGE ( 'NONE', *, *, #21177, .F. ) ;
#19163 = CIRCLE ( 'NONE', #14649, 12.14055452724117856 ) ;
#19164 = VERTEX_POINT ( 'NONE', #22428 ) ;
#19165 = EDGE_CURVE ( 'NONE', #19569, #5921, #18186, .T. ) ;
#19166 = ORIENTED_EDGE ( 'NONE', *, *, #912, .T. ) ;
#19167 = ADVANCED_FACE ( 'NONE', ( #917 ), #15593, .T. ) ;
#19168 = EDGE_CURVE ( 'NONE', #14827, #18651, #11409, .T. ) ;
#19170 = ORIENTED_EDGE ( 'NONE', *, *, #5382, .F. ) ;
#19169 = EDGE_LOOP ( 'NONE', ( #12499, #17005, #20069, #14047 ) ) ;
#19171 = DIRECTION ( 'NONE',  ( -1.000000000000000000, -5.598259082250514647E-17, -3.330669073875432643E-16 ) ) ;
#19172 = DIRECTION ( 'NONE',  ( -2.220446049250313081E-16, 1.000000000000000000, -7.025792437124636392E-31 ) ) ;
#19173 = CARTESIAN_POINT ( 'NONE',  ( 22.49999999999999645, 4.250000000000031974, -1.499999999999997780 ) ) ;
#19174 = ORIENTED_EDGE ( 'NONE', *, *, #12376, .F. ) ;
#19175 = DIRECTION ( 'NONE',  ( 2.013525853228518840E-32, -6.902532920683810383E-31, 1.000000000000000000 ) ) ;
#19176 = DIRECTION ( 'NONE',  ( -1.066786462891689527E-26, -6.656013887802287108E-31, -1.000000000000000000 ) ) ;
#19177 = EDGE_CURVE ( 'NONE', #7460, #23117, #12149, .T. ) ;
#19178 = CARTESIAN_POINT ( 'NONE',  ( -12.84999999999999964, 0.000000000000000000, 0.000000000000000000 ) ) ;
#19179 = CARTESIAN_POINT ( 'NONE',  ( -90.63385214007837476, -2.700000000000084110, -7.926881151201908615 ) ) ;
#19180 = CARTESIAN_POINT ( 'NONE',  ( -6.778475372771961472E-14, -4.736529461165952526, -3.681130640444301605 ) ) ;
#19181 = EDGE_CURVE ( 'NONE', #20452, #22613, #14434, .T. ) ;
#19182 = AXIS2_PLACEMENT_3D ( 'NONE', #11562, #11671, #8391 ) ;
#19183 = CARTESIAN_POINT ( 'NONE',  ( -2.099999999999999645, 2.571758278209440971E-16, -5.294516984716112873 ) ) ;
#19184 = DIRECTION ( 'NONE',  ( 1.550910762415566494E-16, 1.000000000000000000, -8.135128085091684243E-31 ) ) ;
#19185 = DIRECTION ( 'NONE',  ( -1.066605682267576713E-26, 0.000000000000000000, -1.000000000000000000 ) ) ;
#19186 = DIRECTION ( 'NONE',  ( 1.000000000000000000, -2.168404344971005170E-16, 1.203141491611682442E-30 ) ) ;
#19187 = CARTESIAN_POINT ( 'NONE',  ( 4.114405500665258231, -4.051151509359430136, -5.737149237780425473E-18 ) ) ;
#19188 = ORIENTED_EDGE ( 'NONE', *, *, #617, .F. ) ;
#19189 = DIRECTION ( 'NONE',  ( -2.486122532488674318E-16, -6.812994285422901146E-17, -1.000000000000000000 ) ) ;
#19191 = VERTEX_POINT ( 'NONE', #18659 ) ;
#19190 = ORIENTED_EDGE ( 'NONE', *, *, #16958, .T. ) ;
#19192 = UNCERTAINTY_MEASURE_WITH_UNIT (LENGTH_MEASURE( 1.000000000000000082E-05 ), #12532, 'distance_accuracy_value', 'NONE');
#19193 = ORIENTED_EDGE ( 'NONE', *, *, #15551, .F. ) ;
#19195 = ORIENTED_EDGE ( 'NONE', *, *, #23074, .F. ) ;
#19194 = ORIENTED_EDGE ( 'NONE', *, *, #16974, .F. ) ;
#19196 = VECTOR ( 'NONE', #11992, 1000.000000000000000 ) ;
#19197 = TOROIDAL_SURFACE ( 'NONE', #9057, 3.750000000000000000, 1.000000000000000000 ) ;
#19198 = VERTEX_POINT ( 'NONE', #11942 ) ;
#19199 = FACE_OUTER_BOUND ( 'NONE', #20075, .T. ) ;
#19200 = CARTESIAN_POINT ( 'NONE',  ( -4.197393957002396370, -0.8151795401431403132, -3.503767560748964449 ) ) ;
#19201 = DIRECTION ( 'NONE',  ( 0.000000000000000000, 3.382522293539643228E-32, 1.000000000000000000 ) ) ;
#19202 = EDGE_CURVE ( 'NONE', #22242, #343, #2544, .T. ) ;
#19203 = LINE ( 'NONE', #17546, #12031 ) ;
#19204 = DIRECTION ( 'NONE',  ( 1.066786462891689527E-26, 6.656013887802287108E-31, 1.000000000000000000 ) ) ;
#19205 = CARTESIAN_POINT ( 'NONE',  ( 2.775557561562891351E-14, 11.00000000000000000, -6.499999999999950262 ) ) ;
#19206 = FACE_OUTER_BOUND ( 'NONE', #17929, .T. ) ;
#19207 = EDGE_CURVE ( 'NONE', #2089, #7096, #21195, .T. ) ;
#19208 = LINE ( 'NONE', #6405, #3174 ) ;
#19209 = EDGE_CURVE ( 'NONE', #8301, #2644, #20446, .T. ) ;
#19210 = FACE_OUTER_BOUND ( 'NONE', #5436, .T. ) ;
#19211 = FACE_OUTER_BOUND ( 'NONE', #2440, .T. ) ;
#19212 = AXIS2_PLACEMENT_3D ( 'NONE', #14445, #3619, #21627 ) ;
#19213 = COLOUR_RGB ( '', 0.09019608, 0.27058824, 0.51372549) ;
#19214 = CARTESIAN_POINT ( 'NONE',  ( -3.999999999998684164, 1.677772373332598210, -3.535253723897363365 ) ) ;
#19215 = CARTESIAN_POINT ( 'NONE',  ( 4.158921614371306141, -1.986121848748765073, 3.559936047944500359 ) ) ;
#19216 = ORIENTED_EDGE ( 'NONE', *, *, #5369, .F. ) ;
#19217 =( NAMED_UNIT ( * ) SI_UNIT ( $, .STERADIAN. ) SOLID_ANGLE_UNIT ( ) );
#19219 = VERTEX_POINT ( 'NONE', #22550 ) ;
#19218 = ORIENTED_EDGE ( 'NONE', *, *, #336, .F. ) ;
#19220 = EDGE_LOOP ( 'NONE', ( #20354, #19876, #16594, #9972, #6267, #4399 ) ) ;
#19221 = ORIENTED_EDGE ( 'NONE', *, *, #14439, .T. ) ;
#19222 = B_SPLINE_CURVE_WITH_KNOTS ( 'NONE', 3,
 ( #13021, #561, #1370, #13720 ),
 .UNSPECIFIED., .F., .F.,
 ( 4, 4 ),
 ( 6.992893892674702526E-18, 1.060678621364840933E-05 ),
 .UNSPECIFIED. ) ;
#19223 = VERTEX_POINT ( 'NONE', #7957 ) ;
#19224 = FACE_OUTER_BOUND ( 'NONE', #10594, .T. ) ;
#19225 = CIRCLE ( 'NONE', #1941, 2.250000000000003109 ) ;
#19226 = VECTOR ( 'NONE', #18924, 1000.000000000000000 ) ;
#19227 = CARTESIAN_POINT ( 'NONE',  ( 0.1381419387168374702, -1.355287006802384342, 3.499999999999959588 ) ) ;
#19228 = ORIENTED_EDGE ( 'NONE', *, *, #18805, .T. ) ;
#19229 = CARTESIAN_POINT ( 'NONE',  ( -8.718376657154855991, -13.50000000000003553, 6.820622386032004769 ) ) ;
#19230 = DIRECTION ( 'NONE',  ( -1.000000000000000000, 4.981134552447635210E-14, -3.717264591378832268E-16 ) ) ;
#19231 = CARTESIAN_POINT ( 'NONE',  ( 4.000000000000003553, 0.000000000000000000, -5.600000000000000533 ) ) ;
#19232 = DIRECTION ( 'NONE',  ( 1.000000000000000000, 0.000000000000000000, 0.000000000000000000 ) ) ;
#19233 = FACE_OUTER_BOUND ( 'NONE', #22062, .T. ) ;
#19234 = CARTESIAN_POINT ( 'NONE',  ( -0.4634555469063539879, -1.750000000000002220, 4.749999999999999112 ) ) ;
#19235 = DIRECTION ( 'NONE',  ( 2.013525853228518840E-32, -6.902532920683810383E-31, 1.000000000000000000 ) ) ;
#19236 = CARTESIAN_POINT ( 'NONE',  ( 4.330127018922095949, 4.689110867544643568, -7.500000000000003553 ) ) ;
#19237 = CARTESIAN_POINT ( 'NONE',  ( 2.500000000000025313, -2.885729496010498622E-15, -4.974600000000002353 ) ) ;
#19238 = DIRECTION ( 'NONE',  ( 1.000000000000000000, -1.550910762415513985E-16, -3.012982189080959477E-32 ) ) ;
#19239 = ORIENTED_EDGE ( 'NONE', *, *, #17135, .F. ) ;
#19240 = CARTESIAN_POINT ( 'NONE',  ( -90.55603112840530855, 4.857225732735059864E-14, -7.432974388601742533 ) ) ;
#19241 = PLANE ( 'NONE',  #674 ) ;
#19242 = VECTOR ( 'NONE', #5026, 1000.000000000000000 ) ;
#19244 = EDGE_LOOP ( 'NONE', ( #18671, #19312, #20715, #15910 ) ) ;
#19243 = VERTEX_POINT ( 'NONE', #6555 ) ;
#19245 = AXIS2_PLACEMENT_3D ( 'NONE', #95, #16303, #14774 ) ;
#19246 = AXIS2_PLACEMENT_3D ( 'NONE', #19962, #6074, #14660 ) ;
#19247 = ADVANCED_FACE ( 'NONE', ( #6434 ), #12543, .T. ) ;
#19248 = EDGE_LOOP ( 'NONE', ( #6185, #11660, #22579, #1698, #21818 ) ) ;
#19249 = PRODUCT_DEFINITION_SHAPE ( 'NONE', 'NONE',  #11058 ) ;
#19250 = ORIENTED_EDGE ( 'NONE', *, *, #15588, .T. ) ;
#19251 = CARTESIAN_POINT ( 'NONE',  ( 4.580847626786062499, 1.750000000000000222, -1.565739168675242210 ) ) ;
#19252 = DIRECTION ( 'NONE',  ( 0.2405376366294452728, 0.000000000000000000, -0.9706398123736327266 ) ) ;
#19253 = CIRCLE ( 'NONE', #20513, 0.4999999999999994449 ) ;
#19254 = CARTESIAN_POINT ( 'NONE',  ( 63.82609305959173440, -6.614286113036355275, 6.000000000000095923 ) ) ;
#19255 = CARTESIAN_POINT ( 'NONE',  ( 2.742413778650726108, -1.325747111984059590, 4.749999999999997335 ) ) ;
#19256 = CARTESIAN_POINT ( 'NONE',  ( -4.857225732735059864E-14, 4.999999999999976907, -7.500000000000003553 ) ) ;
#19257 = CARTESIAN_POINT ( 'NONE',  ( -5.523909222218111204, 35.99999999900384751, -19.02619312440723576 ) ) ;
#19258 = VECTOR ( 'NONE', #20400, 1000.000000000000000 ) ;
#19259 = CARTESIAN_POINT ( 'NONE',  ( 3.880206590543155531, 2.665671387532511982, 2.382921720510903452 ) ) ;
#19260 = CARTESIAN_POINT ( 'NONE',  ( -7.876571740167083391, -0.1939399797844225393, 7.785394814390953044 ) ) ;
#19261 = AXIS2_PLACEMENT_3D ( 'NONE', #22537, #8300, #22417 ) ;
#19262 = AXIS2_PLACEMENT_3D ( 'NONE', #22333, #22213, #20810 ) ;
#19263 = DIRECTION ( 'NONE',  ( 0.000000000000000000, -3.469446951953616555E-15, -1.000000000000000000 ) ) ;
#19264 = DIRECTION ( 'NONE',  ( 1.000000000000000000, 2.168404344970995063E-16, 6.201636426617045919E-15 ) ) ;
#19265 = FACE_OUTER_BOUND ( 'NONE', #13923, .T. ) ;
#19266 = CARTESIAN_POINT ( 'NONE',  ( -6.999999999708156118, 6.999999999003851947, -15.99999999999999289 ) ) ;
#19267 = B_SPLINE_CURVE_WITH_KNOTS ( 'NONE', 3,
 ( #17113, #19018, #8195, #914, #675, #3014, #6080, #22318 ),
 .UNSPECIFIED., .F., .F.,
 ( 4, 2, 2, 4 ),
 ( 0.005725059856848725010, 0.006314084072593702072, 0.006903108288338679135, 0.008081156719828633261 ),
 .UNSPECIFIED. ) ;
#19268 = CARTESIAN_POINT ( 'NONE',  ( 3.061616997868385113E-16, 1.750000000000001554, 2.500000000000000000 ) ) ;
#19269 = ADVANCED_FACE ( 'NONE', ( #8311 ), #4652, .T. ) ;
#19270 = DIRECTION ( 'NONE',  ( 0.000000000000000000, 0.000000000000000000, -1.000000000000000000 ) ) ;
#19271 = ORIENTED_EDGE ( 'NONE', *, *, #17280, .F. ) ;
#19272 = EDGE_CURVE ( 'NONE', #11088, #10365, #20904, .T. ) ;
#19273 = CIRCLE ( 'NONE', #8754, 6.249999999999992006 ) ;
#19274 = EDGE_LOOP ( 'NONE', ( #4136, #18469, #18475, #13116 ) ) ;
#19275 = AXIS2_PLACEMENT_3D ( 'NONE', #1983, #12580, #10811 ) ;
#19276 = CIRCLE ( 'NONE', #5005, 4.000000000000045297 ) ;
#19277 = CIRCLE ( 'NONE', #1996, 0.5000000000000029976 ) ;
#19278 = CARTESIAN_POINT ( 'NONE',  ( -5.311293330707327343, 35.99999999900384751, -25.93870558608502463 ) ) ;
#19279 = VECTOR ( 'NONE', #9426, 1000.000000000000000 ) ;
#19282 = ORIENTED_EDGE ( 'NONE', *, *, #9572, .T. ) ;
#19281 = ADVANCED_FACE ( 'NONE', ( #3598 ), #10292, .F. ) ;
#19280 = VERTEX_POINT ( 'NONE', #19237 ) ;
#19283 = EDGE_CURVE ( 'NONE', #7855, #21664, #4883, .T. ) ;
#19284 = DIRECTION ( 'NONE',  ( 0.000000000000000000, 0.000000000000000000, 1.000000000000000000 ) ) ;
#19285 = EDGE_CURVE ( 'NONE', #9040, #9710, #21491, .T. ) ;
#19286 = EDGE_LOOP ( 'NONE', ( #4860, #19542, #663, #4645 ) ) ;
#19287 = CARTESIAN_POINT ( 'NONE',  ( 2.081668171172168513E-14, 10.00000000000000533, 0.000000000000000000 ) ) ;
#19288 = ORIENTED_EDGE ( 'NONE', *, *, #21581, .F. ) ;
#19289 = CARTESIAN_POINT ( 'NONE',  ( -50.65685424949274562, 7.199999999999935341, -8.000000000000062172 ) ) ;
#19290 = CARTESIAN_POINT ( 'NONE',  ( -43.10883117545719045, 4.565685424949256443, 7.500000000000007105 ) ) ;
#19291 = LINE ( 'NONE', #13998, #5300 ) ;
#19292 = DIRECTION ( 'NONE',  ( 0.7313537016191730133, -0.6819983600624958120, 5.924440990721418971E-17 ) ) ;
#19293 = CARTESIAN_POINT ( 'NONE',  ( 42.50000000000020606, 8.500000000000003553, -13.00000000000002487 ) ) ;
#19294 = TOROIDAL_SURFACE ( 'NONE', #21582, 3.750000000000000000, 1.000000000000000000 ) ;
#19295 = AXIS2_PLACEMENT_3D ( 'NONE', #3595, #7473, #10873 ) ;
#19296 = CARTESIAN_POINT ( 'NONE',  ( -6.746326818733273001, -2.700000000000056577, 27.22340457528592239 ) ) ;
#19297 = VECTOR ( 'NONE', #15493, 1000.000000000000000 ) ;
#19298 = DIRECTION ( 'NONE',  ( 1.000000000000000000, -1.734723475976793289E-15, -1.319263693449169988E-31 ) ) ;
#19299 = VECTOR ( 'NONE', #11123, 1000.000000000000000 ) ;
#19300 = SURFACE_STYLE_FILL_AREA ( #12110 ) ;
#19301 = EDGE_CURVE ( 'NONE', #13876, #1919, #6546, .T. ) ;
#19302 = VECTOR ( 'NONE', #20011, 1000.000000000000000 ) ;
#19303 = ADVANCED_FACE ( 'NONE', ( #7022 ), #12050, .F. ) ;
#19304 = ADVANCED_FACE ( 'NONE', ( #8656 ), #537, .F. ) ;
#19305 = CARTESIAN_POINT ( 'NONE',  ( 2.775557561562891351E-14, 2.499999999999995115, -12.50000000000001066 ) ) ;
#19306 = ORIENTED_EDGE ( 'NONE', *, *, #18726, .F. ) ;
#19308 = ORIENTED_EDGE ( 'NONE', *, *, #6870, .F. ) ;
#19307 = ORIENTED_EDGE ( 'NONE', *, *, #12230, .F. ) ;
#19309 = ADVANCED_FACE ( 'NONE', ( #14070 ), #10648, .F. ) ;
#19310 = EDGE_LOOP ( 'NONE', ( #21290, #689, #1915, #13362 ) ) ;
#19311 = AXIS2_PLACEMENT_3D ( 'NONE', #4122, #16701, #20364 ) ;
#19314 = ORIENTED_EDGE ( 'NONE', *, *, #1345, .F. ) ;
#19313 = EDGE_CURVE ( 'NONE', #1694, #6466, #19721, .T. ) ;
#19312 = ORIENTED_EDGE ( 'NONE', *, *, #17582, .F. ) ;
#19315 = AXIS2_PLACEMENT_3D ( 'NONE', #22750, #14036, #17439 ) ;
#19316 = EDGE_LOOP ( 'NONE', ( #3188, #3265, #18417 ) ) ;
#19317 = DIRECTION ( 'NONE',  ( -8.438582421954109416E-32, 0.000000000000000000, -1.000000000000000000 ) ) ;
#19318 = AXIS2_PLACEMENT_3D ( 'NONE', #22304, #13929, #21003 ) ;
#19319 = EDGE_CURVE ( 'NONE', #4569, #9677, #13292, .T. ) ;
#19320 = DIRECTION ( 'NONE',  ( 4.190823558986625216E-31, -1.000000000000000000, 4.190823558986625216E-31 ) ) ;
#19321 = DIRECTION ( 'NONE',  ( -0.000000000000000000, 1.000000000000000000, -0.000000000000000000 ) ) ;
#19322 = CYLINDRICAL_SURFACE ( 'NONE', #7220, 6.999999999999999112 ) ;
#19323 = DIRECTION ( 'NONE',  ( 0.000000000000000000, 0.000000000000000000, 1.000000000000000000 ) ) ;
#19324 = EDGE_CURVE ( 'NONE', #18733, #5138, #18789, .T. ) ;
#19325 = CARTESIAN_POINT ( 'NONE',  ( -7.473326079327731186, -0.1514770120355157235, 7.598194856234254502 ) ) ;
#19326 = CARTESIAN_POINT ( 'NONE',  ( 4.690415759823387987, 0.7500000000000492939, -3.000000000000002665 ) ) ;
#19327 = DIRECTION ( 'NONE',  ( -2.013525853228507892E-32, -6.902532920683810383E-31, 1.000000000000000000 ) ) ;
#19328 = CARTESIAN_POINT ( 'NONE',  ( -2.099999999999999645, 2.571758278209440971E-16, -5.600000000000000533 ) ) ;
#19329 = CARTESIAN_POINT ( 'NONE',  ( 77.42435809754141474, -4.499999999999809930, 6.000000000000095923 ) ) ;
#19330 = DIRECTION ( 'NONE',  ( 3.254448077146059901E-32, 1.000000000000000000, 6.409494854920712161E-31 ) ) ;
#19331 = CARTESIAN_POINT ( 'NONE',  ( 4.692963726980105221, 1.672424706883761658, 1.371548386792669438 ) ) ;
#19332 = VECTOR ( 'NONE', #9521, 1000.000000000000000 ) ;
#19333 = EDGE_CURVE ( 'NONE', #8988, #4062, #19692, .T. ) ;
#19334 = CLOSED_SHELL ( 'NONE', ( #6343, #14156, #20188, #13934, #6923, #1207, #23175, #1198, #21663, #6260, #22807, #19080, #21319 ) ) ;
#19335 = CARTESIAN_POINT ( 'NONE',  ( 24.75000000000001066, 2.000000000000099032, -16.99999999999999289 ) ) ;
#19336 = DIRECTION ( 'NONE',  ( 0.000000000000000000, 0.000000000000000000, -1.000000000000000000 ) ) ;
#19337 = CARTESIAN_POINT ( 'NONE',  ( 77.42435809754135789, -10.99999999999981526, 6.500000000000123457 ) ) ;
#19338 = ORIENTED_EDGE ( 'NONE', *, *, #3964, .T. ) ;
#19340 = EDGE_LOOP ( 'NONE', ( #15016, #6631, #11573, #1918 ) ) ;
#19339 = ORIENTED_EDGE ( 'NONE', *, *, #12401, .T. ) ;
#19341 = EDGE_CURVE ( 'NONE', #5825, #19191, #7537, .T. ) ;
#19342 = ORIENTED_EDGE ( 'NONE', *, *, #3481, .T. ) ;
#19343 = ORIENTED_EDGE ( 'NONE', *, *, #17273, .F. ) ;
#19344 = EDGE_CURVE ( 'NONE', #12739, #16509, #4273, .T. ) ;
#19345 = ORIENTED_EDGE ( 'NONE', *, *, #2903, .F. ) ;
#19346 = ORIENTED_EDGE ( 'NONE', *, *, #7716, .F. ) ;
#19347 = DIRECTION ( 'NONE',  ( 0.000000000000000000, 0.000000000000000000, 1.000000000000000000 ) ) ;
#19348 = VECTOR ( 'NONE', #941, 1000.000000000000000 ) ;
#19349 = FACE_OUTER_BOUND ( 'NONE', #4674, .T. ) ;
#19350 = ORIENTED_EDGE ( 'NONE', *, *, #4369, .F. ) ;
#19351 = DIRECTION ( 'NONE',  ( -5.598259082250514647E-17, 1.000000000000000000, -6.162975822039315660E-32 ) ) ;
#19352 = PLANE ( 'NONE',  #10610 ) ;
#19353 = CARTESIAN_POINT ( 'NONE',  ( -0.6920835326022843903, -4.454600218803954625, -3.597382984111614945 ) ) ;
#19354 = DIRECTION ( 'NONE',  ( 0.000000000000000000, 0.000000000000000000, -1.000000000000000000 ) ) ;
#19355 = CARTESIAN_POINT ( 'NONE',  ( 6.999999999999992006, -8.000000000000010658, 10.74999999999999645 ) ) ;
#19356 = CARTESIAN_POINT ( 'NONE',  ( -6.938893903907228378E-15, -9.999999999999968026, 0.000000000000000000 ) ) ;
#19357 = DIRECTION ( 'NONE',  ( -1.066786462891689527E-26, -6.656013887802287108E-31, -1.000000000000000000 ) ) ;
#19358 = CARTESIAN_POINT ( 'NONE',  ( 0.2500000000000036637, 2.000000000000001776, -17.50000000000000711 ) ) ;
#19359 = FACE_OUTER_BOUND ( 'NONE', #12471, .T. ) ;
#19360 = CARTESIAN_POINT ( 'NONE',  ( -6.999999999708142795, 13.99999999900385106, -19.00000000000000355 ) ) ;
#19361 = DIRECTION ( 'NONE',  ( 3.070652698126927723E-17, 1.000000000000000000, -4.167305704548413124E-17 ) ) ;
#19362 = ORIENTED_EDGE ( 'NONE', *, *, #22942, .F. ) ;
#19363 = CARTESIAN_POINT ( 'NONE',  ( 3.972709601346593011, 2.746729940827194127, -2.374099244652738694 ) ) ;
#19364 = VECTOR ( 'NONE', #3059, 1000.000000000000000 ) ;
#19365 = CARTESIAN_POINT ( 'NONE',  ( 108.2426266706971205, -11.02760560296367487, -6.500000000000075495 ) ) ;
#19367 = VERTEX_POINT ( 'NONE', #14525 ) ;
#19366 = ORIENTED_EDGE ( 'NONE', *, *, #9498, .F. ) ;
#19368 = ADVANCED_FACE ( 'NONE', ( #16282 ), #3156, .T. ) ;
#19369 = ORIENTED_EDGE ( 'NONE', *, *, #12117, .F. ) ;
#19370 = ADVANCED_FACE ( 'NONE', ( #9665 ), #22309, .T. ) ;
#19371 = VERTEX_POINT ( 'NONE', #22251 ) ;
#19372 = FACE_OUTER_BOUND ( 'NONE', #10593, .T. ) ;
#19373 = DIRECTION ( 'NONE',  ( -4.190823558986625216E-31, 1.000000000000000000, -4.190823558986625216E-31 ) ) ;
#19374 = DIRECTION ( 'NONE',  ( 1.000000000000000000, 0.000000000000000000, 0.000000000000000000 ) ) ;
#19375 = LINE ( 'NONE', #6921, #22802 ) ;
#19376 = CARTESIAN_POINT ( 'NONE',  ( -3.999999999708153453, 42.99999999900385461, -29.50000000000000000 ) ) ;
#19377 = CARTESIAN_POINT ( 'NONE',  ( 80.15235153779141797, -8.074585193523137860, -6.500000000000019540 ) ) ;
#19378 = DIRECTION ( 'NONE',  ( -2.013525853228507892E-32, -6.902532920683810383E-31, 1.000000000000000000 ) ) ;
#19379 = CARTESIAN_POINT ( 'NONE',  ( -7.525553787417682550, -1.070926652787118405, 8.786654903594046218 ) ) ;
#19380 = CARTESIAN_POINT ( 'NONE',  ( 30.00000000029184832, 2.999999999003851503, -45.00000000000000000 ) ) ;
#19381 = DIRECTION ( 'NONE',  ( 0.000000000000000000, 6.802837160693368935E-15, 1.000000000000000000 ) ) ;
#19382 = LINE ( 'NONE', #22572, #22466 ) ;
#19383 = CARTESIAN_POINT ( 'NONE',  ( 54.42435809754109499, 0.4999999999999449329, 6.500000000000144773 ) ) ;
#19384 = LINE ( 'NONE', #1849, #13418 ) ;
#19385 = CARTESIAN_POINT ( 'NONE',  ( -8.660254037844428154, 4.689110867544629357, -1.387778780781445676E-14 ) ) ;
#19386 = CIRCLE ( 'NONE', #11483, 3.500000000000023981 ) ;
#19387 = CARTESIAN_POINT ( 'NONE',  ( 54.42435809754106657, -4.000000000000003553, 6.000000000000136779 ) ) ;
#19388 = CARTESIAN_POINT ( 'NONE',  ( 2.742413778650726108, 1.750000000000001554, 4.750000000000000888 ) ) ;
#19389 = VERTEX_POINT ( 'NONE', #16163 ) ;
#19390 = ORIENTED_EDGE ( 'NONE', *, *, #21633, .F. ) ;
#19391 = DIRECTION ( 'NONE',  ( 0.000000000000000000, 0.000000000000000000, 1.000000000000000000 ) ) ;
#19393 = ORIENTED_EDGE ( 'NONE', *, *, #7816, .F. ) ;
#19392 = ORIENTED_EDGE ( 'NONE', *, *, #14791, .F. ) ;
#19394 = CARTESIAN_POINT ( 'NONE',  ( 12.84999999999997300, 0.000000000000000000, 1.387778780781445676E-14 ) ) ;
#19395 = ORIENTED_EDGE ( 'NONE', *, *, #19117, .F. ) ;
#19396 = CARTESIAN_POINT ( 'NONE',  ( 73.50000000000116529, -3.999999999999809042, -2.549999999999874589 ) ) ;
#19397 = SURFACE_STYLE_FILL_AREA ( #5057 ) ;
#19398 = AXIS2_PLACEMENT_3D ( 'NONE', #17474, #19361, #1484 ) ;
#19399 = PRODUCT_RELATED_PRODUCT_CATEGORY ( 'part', '', ( #8169 ) ) ;
#19400 = CARTESIAN_POINT ( 'NONE',  ( 0.000000000000000000, 1.750000000000001554, 0.000000000000000000 ) ) ;
#19401 = ORIENTED_EDGE ( 'NONE', *, *, #21922, .F. ) ;
#19402 = AXIS2_PLACEMENT_3D ( 'NONE', #7248, #20060, #9352 ) ;
#19403 = FACE_OUTER_BOUND ( 'NONE', #1382, .T. ) ;
#19404 = CYLINDRICAL_SURFACE ( 'NONE', #1053, 0.5000000000000038858 ) ;
#19405 = DIRECTION ( 'NONE',  ( 1.733449886265891589E-32, -4.190823558986610327E-31, 1.000000000000000000 ) ) ;
#19406 = CARTESIAN_POINT ( 'NONE',  ( 4.071447262713884463, 4.041451884327383226, 0.000000000000000000 ) ) ;
#19407 = ADVANCED_FACE ( 'NONE', ( #21715 ), #82, .T. ) ;
#19408 = CARTESIAN_POINT ( 'NONE',  ( 37.50000000000016342, 11.00000000000000355, -2.316987298107758164 ) ) ;
#19409 = CARTESIAN_POINT ( 'NONE',  ( 4.170895651974852569, 2.054890354522450835, -3.559174498016476562 ) ) ;
#19410 = CARTESIAN_POINT ( 'NONE',  ( 4.086376042167605860, -1.979461949354230255, 3.571471332069165339 ) ) ;
#19411 =( NAMED_UNIT ( * ) PLANE_ANGLE_UNIT ( ) SI_UNIT ( $, .RADIAN. ) );
#19412 = EDGE_CURVE ( 'NONE', #7030, #16729, #6027, .T. ) ;
#19413 =( NAMED_UNIT ( * ) PLANE_ANGLE_UNIT ( ) SI_UNIT ( $, .RADIAN. ) );
#19414 = EDGE_CURVE ( 'NONE', #14699, #9093, #18557, .T. ) ;
#19415 = ORIENTED_EDGE ( 'NONE', *, *, #11383, .F. ) ;
#19416 = VECTOR ( 'NONE', #15186, 1000.000000000000000 ) ;
#19417 = AXIS2_PLACEMENT_3D ( 'NONE', #15413, #19070, #15644 ) ;
#19418 = CARTESIAN_POINT ( 'NONE',  ( -25.13934240061087166, 60.78549366357398753, 34.16570243528389028 ) ) ;
#19420 = ORIENTED_EDGE ( 'NONE', *, *, #9950, .T. ) ;
#19419 = VERTEX_POINT ( 'NONE', #1931 ) ;
#19421 = VECTOR ( 'NONE', #16700, 1000.000000000000000 ) ;
#19422 = ORIENTED_EDGE ( 'NONE', *, *, #19344, .F. ) ;
#19424 = ORIENTED_EDGE ( 'NONE', *, *, #16971, .T. ) ;
#19423 = EDGE_LOOP ( 'NONE', ( #2265, #5342, #22326, #2142 ) ) ;
#19425 = CARTESIAN_POINT ( 'NONE',  ( 1.274258131565143559, 3.883108878240837392, -3.220599429844244188 ) ) ;
#19426 = CARTESIAN_POINT ( 'NONE',  ( 66.26395429947837101, 0.000000000000000000, -5.999999999999908518 ) ) ;
#19427 = EDGE_CURVE ( 'NONE', #7622, #16517, #12640, .T. ) ;
#19428 = CYLINDRICAL_SURFACE ( 'NONE', #14702, 0.5000000000000038858 ) ;
#19429 = LINE ( 'NONE', #1555, #23197 ) ;
#19430 = CYLINDRICAL_SURFACE ( 'NONE', #9777, 0.5000000000000022204 ) ;
#19431 = DIRECTION ( 'NONE',  ( -4.019602852144215652E-47, -6.982962677686261977E-15, -1.000000000000000000 ) ) ;
#19432 = VECTOR ( 'NONE', #10795, 1000.000000000000000 ) ;
#19433 = EDGE_CURVE ( 'NONE', #1550, #12680, #13325, .T. ) ;
#19434 = DIRECTION ( 'NONE',  ( -8.438582421954109416E-32, 0.000000000000000000, -1.000000000000000000 ) ) ;
#19435 = DIRECTION ( 'NONE',  ( -1.000000000000000000, -3.254448077276381206E-32, -1.066788928082016908E-26 ) ) ;
#19436 = CARTESIAN_POINT ( 'NONE',  ( -6.950726493550218217E-14, 4.999999999999976907, -4.750000000000041744 ) ) ;
#19437 = LINE ( 'NONE', #2020, #906 ) ;
#19438 = CIRCLE ( 'NONE', #17572, 1.000000000000000000 ) ;
#19439 = CARTESIAN_POINT ( 'NONE',  ( -43.10883117545719045, 4.565685424949256443, 7.500000000000007105 ) ) ;
#19440 = CARTESIAN_POINT ( 'NONE',  ( 5.484827557301438894, 1.325747111984056037, 0.000000000000000000 ) ) ;
#19441 = AXIS2_PLACEMENT_3D ( 'NONE', #7448, #10852, #16248 ) ;
#19442 = EDGE_CURVE ( 'NONE', #22993, #14621, #16710, .T. ) ;
#19443 = DIRECTION ( 'NONE',  ( -1.000000000000000000, 1.550910762415513985E-16, 3.012982189080959477E-32 ) ) ;
#19444 = ADVANCED_FACE ( 'NONE', ( #618 ), #11536, .T. ) ;
#19445 = CARTESIAN_POINT ( 'NONE',  ( -4.000000000000103029, 1.700094919196693644, -3.320312364301530206 ) ) ;
#19446 = DIRECTION ( 'NONE',  ( 1.000000000000000000, 4.780126911580487002E-14, 3.854941057726199147E-16 ) ) ;
#19447 = PRODUCT ( 'Bolt', 'Bolt', '', ( #12944 ) ) ;
#19448 = AXIS2_PLACEMENT_3D ( 'NONE', #11452, #14876, #5716 ) ;
#19449 = ORIENTED_EDGE ( 'NONE', *, *, #13056, .T. ) ;
#19450 = SHAPE_REPRESENTATION ( 'MAS-693', ( #11258, #3002, #17261, #18040, #9765, #19918, #6010, #22927, #8261, #15382, #18399, #21423, #12771, #9385, #16500, #7882, #6384, #10504, #13516, #19523, #22534 ), #1494 ) ;
#19452 = ORIENTED_EDGE ( 'NONE', *, *, #5944, .F. ) ;
#19451 = EDGE_LOOP ( 'NONE', ( #1855, #18874, #13837, #14565 ) ) ;
#19453 = CIRCLE ( 'NONE', #16433, 4.000000000000045297 ) ;
#19454 = ORIENTED_EDGE ( 'NONE', *, *, #15455, .T. ) ;
#19455 = ORIENTED_EDGE ( 'NONE', *, *, #11801, .T. ) ;
#19457 = VERTEX_POINT ( 'NONE', #13196 ) ;
#19456 = EDGE_CURVE ( 'NONE', #13386, #8317, #7900, .T. ) ;
#19458 = EDGE_CURVE ( 'NONE', #17239, #17095, #1940, .T. ) ;
#19459 = EDGE_LOOP ( 'NONE', ( #17712, #23180 ) ) ;
#19460 = EDGE_CURVE ( 'NONE', #1004, #19811, #11198, .T. ) ;
#19461 = DIRECTION ( 'NONE',  ( 7.860214984771176937E-18, 1.409037165336591006E-16, 1.000000000000000000 ) ) ;
#19462 = VECTOR ( 'NONE', #11977, 1000.000000000000000 ) ;
#19463 = ADVANCED_FACE ( 'NONE', ( #15060, #16324 ), #9928, .F. ) ;
#19464 = VECTOR ( 'NONE', #22112, 1000.000000000000000 ) ;
#19465 = AXIS2_PLACEMENT_3D ( 'NONE', #2778, #20547, #13368 ) ;
#19466 = DIRECTION ( 'NONE',  ( -0.1556420233463030045, -1.387778780781374185E-17, -0.9878135252003127365 ) ) ;
#19467 = ORIENTED_EDGE ( 'NONE', *, *, #6670, .F. ) ;
#19468 = LINE ( 'NONE', #6763, #10881 ) ;
#19469 = CARTESIAN_POINT ( 'NONE',  ( 0.000000000000000000, -1.750000000000001554, 0.000000000000000000 ) ) ;
#19470 = DIRECTION ( 'NONE',  ( 1.000000000000000000, -7.100545512326564696E-57, -1.066786462891689527E-26 ) ) ;
#19471 = DIRECTION ( 'NONE',  ( 0.000000000000000000, -1.000000000000000000, 0.000000000000000000 ) ) ;
#19472 = CARTESIAN_POINT ( 'NONE',  ( 27.94974746859769255, 27.94974746730969528, -25.50000000000000355 ) ) ;
#19473 = EDGE_CURVE ( 'NONE', #21954, #6421, #10153, .T. ) ;
#19474 = CARTESIAN_POINT ( 'NONE',  ( -6.960550854630938034, 36.00005224601466836, -26.48493219021591827 ) ) ;
#19475 = VECTOR ( 'NONE', #18962, 1000.000000000000000 ) ;
#19476 = DIRECTION ( 'NONE',  ( 0.000000000000000000, 0.000000000000000000, -1.000000000000000000 ) ) ;
#19477 = CARTESIAN_POINT ( 'NONE',  ( 30.00000000029184832, 2.999999999003851503, -8.549999999999997158 ) ) ;
#19478 = ADVANCED_FACE ( 'NONE', ( #22625 ), #15923, .T. ) ;
#19479 = DIRECTION ( 'NONE',  ( 1.000000000000000000, -4.190823558986610327E-31, 1.733449886265890494E-32 ) ) ;
#19480 = CARTESIAN_POINT ( 'NONE',  ( 12.49999999999995914, 2.775557561562891351E-14, -9.500000000000003553 ) ) ;
#19481 = EDGE_CURVE ( 'NONE', #18229, #10215, #8959, .T. ) ;
#19482 = VERTEX_POINT ( 'NONE', #17437 ) ;
#19483 = CIRCLE ( 'NONE', #16458, 0.5000000000000022204 ) ;
#19484 = PLANE ( 'NONE',  #2595 ) ;
#19485 = CIRCLE ( 'NONE', #1091, 4.000000000000045297 ) ;
#19486 = CARTESIAN_POINT ( 'NONE',  ( 81.04599508018866061, -4.805938895142331191, -5.999999999999950262 ) ) ;
#19487 = AXIS2_PLACEMENT_3D ( 'NONE', #12875, #14521, #2400 ) ;
#19489 = ORIENTED_EDGE ( 'NONE', *, *, #2965, .F. ) ;
#19488 = EDGE_LOOP ( 'NONE', ( #22389, #10714, #23142, #575 ) ) ;
#19490 = ORIENTED_EDGE ( 'NONE', *, *, #16005, .T. ) ;
#19491 = ORIENTED_EDGE ( 'NONE', *, *, #877, .F. ) ;
#19492 = DIRECTION ( 'NONE',  ( -1.000000000000000000, 1.060108790874707909E-14, 0.000000000000000000 ) ) ;
#19493 = CARTESIAN_POINT ( 'NONE',  ( 42.00000000000012079, 0.5000000000000004441, -12.49999999999999645 ) ) ;
#19494 = AXIS2_PLACEMENT_3D ( 'NONE', #836, #13070, #4118 ) ;
#19495 = CARTESIAN_POINT ( 'NONE',  ( 8.137537312224758068, -0.5625089224579603586, 7.396067884835346717 ) ) ;
#19496 = DIRECTION ( 'NONE',  ( 1.000000000000000000, -1.389842848855773367E-62, 2.013525853228507892E-32 ) ) ;
#19497 = DIRECTION ( 'NONE',  ( 2.172745813409349776E-17, -1.000000000000000000, 1.309377075419428048E-16 ) ) ;
#19498 = VECTOR ( 'NONE', #5009, 1000.000000000000114 ) ;
#19499 = DIRECTION ( 'NONE',  ( 0.000000000000000000, 0.000000000000000000, 1.000000000000000000 ) ) ;
#19500 = CARTESIAN_POINT ( 'NONE',  ( 12.84999999999997300, -12.00000000000006928, 4.163336342344337027E-14 ) ) ;
#19501 = AXIS2_PLACEMENT_3D ( 'NONE', #22075, #13140, #14543 ) ;
#19502 = CARTESIAN_POINT ( 'NONE',  ( -8.697224362267961695, 1.160096324559489744E-14, 6.249999999999961808 ) ) ;
#19503 = EDGE_CURVE ( 'NONE', #2067, #5016, #20466, .T. ) ;
#19504 = FACE_OUTER_BOUND ( 'NONE', #11897, .T. ) ;
#19505 = CARTESIAN_POINT ( 'NONE',  ( 12.84999999999997300, -12.00000000000006928, 4.163336342344337027E-14 ) ) ;
#19506 = CARTESIAN_POINT ( 'NONE',  ( 37.35148779274808817, 10.63811079452496422, -10.35148779274853936 ) ) ;
#19507 = LINE ( 'NONE', #12319, #6136 ) ;
#19508 = DIRECTION ( 'NONE',  ( 2.172745813409348851E-17, -1.000000000000000000, -3.406761633869148826E-16 ) ) ;
#19509 = FACE_OUTER_BOUND ( 'NONE', #6883, .T. ) ;
#19510 = ADVANCED_FACE ( 'NONE', ( #12141 ), #6282, .F. ) ;
#19511 =( GEOMETRIC_REPRESENTATION_CONTEXT ( 3 ) GLOBAL_UNCERTAINTY_ASSIGNED_CONTEXT ( ( #22289 ) ) GLOBAL_UNIT_ASSIGNED_CONTEXT ( ( #17812, #8631, #12150 ) ) REPRESENTATION_CONTEXT ( 'NONE', 'WORKASPACE' ) );
#19512 = DIRECTION ( 'NONE',  ( 1.000000000000000000, -1.276756478318923119E-15, -1.333893503340774882E-15 ) ) ;
#19513 = DIRECTION ( 'NONE',  ( -1.000000000000000000, -6.224605580259554159E-31, 2.887593071917436153E-31 ) ) ;
#19514 = ORIENTED_EDGE ( 'NONE', *, *, #9500, .T. ) ;
#19515 = AXIS2_PLACEMENT_3D ( 'NONE', #12483, #14033, #8735 ) ;
#19516 = VERTEX_POINT ( 'NONE', #1113 ) ;
#19517 = CARTESIAN_POINT ( 'NONE',  ( -6.566827242015937038, 35.99999999936095207, -26.31323010872985435 ) ) ;
#19519 = EDGE_LOOP ( 'NONE', ( #10856, #5981, #12326, #17965 ) ) ;
#19518 = ORIENTED_EDGE ( 'NONE', *, *, #3266, .F. ) ;
#19520 = AXIS2_PLACEMENT_3D ( 'NONE', #3186, #3302, #17516 ) ;
#19521 = CARTESIAN_POINT ( 'NONE',  ( 35.50000000029185543, 16.99999999900385461, -19.00000000000000355 ) ) ;
#19522 = CARTESIAN_POINT ( 'NONE',  ( 2.171643655288359565, -3.365003104552389157, -3.921216680110290851E-14 ) ) ;
#19523 = AXIS2_PLACEMENT_3D ( 'NONE', #6973, #17898, #13784 ) ;
#19524 = PLANE ( 'NONE',  #21635 ) ;
#19525 = DIRECTION ( 'NONE',  ( -5.551115123125782702E-16, -2.146163712481653435E-16, 1.000000000000000000 ) ) ;
#19526 = ORIENTED_EDGE ( 'NONE', *, *, #13961, .F. ) ;
#19527 = CARTESIAN_POINT ( 'NONE',  ( -89.70000000000054285, -0.5000000000000628386, 1.000000000000000888 ) ) ;
#19528 = CARTESIAN_POINT ( 'NONE',  ( 0.2182387239012278379, 1.693823289460844927, 3.499999999999957812 ) ) ;
#19529 = CARTESIAN_POINT ( 'NONE',  ( 0.000000000000000000, 0.000000000000000000, 0.000000000000000000 ) ) ;
#19530 = DIRECTION ( 'NONE',  ( -2.013525853228507892E-32, -6.902532920683810383E-31, 1.000000000000000000 ) ) ;
#19531 = DIRECTION ( 'NONE',  ( -1.000000000000000000, 0.000000000000000000, 0.000000000000000000 ) ) ;
#19532 = CARTESIAN_POINT ( 'NONE',  ( -12.85000000000001386, 0.000000000000000000, -5.749999999999991118 ) ) ;
#19533 = DIRECTION ( 'NONE',  ( 1.000000000000000000, -4.440892098500650814E-16, -7.860214984771113767E-18 ) ) ;
#19534 = DIRECTION ( 'NONE',  ( -1.000000000000000000, 1.550910762415500426E-16, 0.000000000000000000 ) ) ;
#19535 = CARTESIAN_POINT ( 'NONE',  ( -12.84999999999999964, -13.50000000000003020, 5.750000000000032863 ) ) ;
#19536 = CONICAL_SURFACE ( 'NONE', #4499, 4.000000000000022204, 0.8911886515913840512 ) ;
#19537 = CARTESIAN_POINT ( 'NONE',  ( 4.151274195509685683, -4.079825909417488461, 1.030604039451950803E-15 ) ) ;
#19538 = PRODUCT_DEFINITION_FORMATION_WITH_SPECIFIED_SOURCE ( 'ANY', '', #12303, .NOT_KNOWN. ) ;
#19539 = ORIENTED_EDGE ( 'NONE', *, *, #10256, .F. ) ;
#19540 =( NAMED_UNIT ( * ) PLANE_ANGLE_UNIT ( ) SI_UNIT ( $, .RADIAN. ) );
#19542 = ORIENTED_EDGE ( 'NONE', *, *, #4338, .T. ) ;
#19541 = ORIENTED_EDGE ( 'NONE', *, *, #7294, .T. ) ;
#19543 = EDGE_CURVE ( 'NONE', #9718, #172, #6621, .T. ) ;
#19544 = ORIENTED_EDGE ( 'NONE', *, *, #5954, .F. ) ;
#19546 = ORIENTED_EDGE ( 'NONE', *, *, #7849, .F. ) ;
#19545 = EDGE_LOOP ( 'NONE', ( #22411, #8667, #22058, #13732 ) ) ;
#19547 = CARTESIAN_POINT ( 'NONE',  ( 2.756197834949904557, 3.027510591568840503, -3.223146290109631718 ) ) ;
#19548 = DIRECTION ( 'NONE',  ( -0.7453559924999295649, 0.000000000000000000, 0.6666666666666669627 ) ) ;
#19549 = FILL_AREA_STYLE ('',( #1438 ) ) ;
#19550 = DIRECTION ( 'NONE',  ( -0.7071067811865505703, 0.7071067811865447972, -1.952833229202414720E-15 ) ) ;
#19551 = FACE_OUTER_BOUND ( 'NONE', #10086, .T. ) ;
#19552 = CARTESIAN_POINT ( 'NONE',  ( -7.126417736726627261, -0.4330224014298838520, 8.494066294656311911 ) ) ;
#19553 = DIRECTION ( 'NONE',  ( 0.000000000000000000, 0.000000000000000000, 1.000000000000000000 ) ) ;
#19554 = CYLINDRICAL_SURFACE ( 'NONE', #5252, 6.249999999999992006 ) ;
#19555 = FACE_OUTER_BOUND ( 'NONE', #4108, .T. ) ;
#19556 = CARTESIAN_POINT ( 'NONE',  ( -55.25320565519145788, 1.040834085586084257E-13, 10.00000000000009237 ) ) ;
#19557 = DIRECTION ( 'NONE',  ( 1.000000000000000000, -4.615739097524200579E-16, 0.000000000000000000 ) ) ;
#19558 = EDGE_CURVE ( 'NONE', #10053, #6092, #8119, .T. ) ;
#19559 = DIRECTION ( 'NONE',  ( 1.000000000000000000, -4.437342591868175641E-31, 3.330669073875457788E-16 ) ) ;
#19560 = DIRECTION ( 'NONE',  ( 0.8571428571428572063, -1.183291357831519285E-30, 0.5150787536377126052 ) ) ;
#19561 = ADVANCED_BREP_SHAPE_REPRESENTATION ( '', ( #13352, #22115 ), #17228 ) ;
#19562 = DIRECTION ( 'NONE',  ( -0.000000000000000000, 1.000000000000000000, -0.000000000000000000 ) ) ;
#19563 = CARTESIAN_POINT ( 'NONE',  ( -4.000000000000106581, -0.8382240730042997967, -3.220610619766981930 ) ) ;
#19564 = CARTESIAN_POINT ( 'NONE',  ( 4.158806965674306078, -4.075748668183979184, -0.05940377217583765745 ) ) ;
#19565 = VERTEX_POINT ( 'NONE', #3223 ) ;
#19566 = ADVANCED_FACE ( 'NONE', ( #20872 ), #20754, .F. ) ;
#19567 =( NAMED_UNIT ( * ) PLANE_ANGLE_UNIT ( ) SI_UNIT ( $, .RADIAN. ) );
#19569 = VERTEX_POINT ( 'NONE', #4851 ) ;
#19568 = ORIENTED_EDGE ( 'NONE', *, *, #16575, .T. ) ;
#19570 = EDGE_CURVE ( 'NONE', #4397, #20741, #9934, .T. ) ;
#19571 = ORIENTED_EDGE ( 'NONE', *, *, #8222, .T. ) ;
#19573 = ORIENTED_EDGE ( 'NONE', *, *, #5351, .F. ) ;
#19572 = VERTEX_POINT ( 'NONE', #18855 ) ;
#19574 = EDGE_LOOP ( 'NONE', ( #15018, #22473, #18730, #23240 ) ) ;
#19575 = EDGE_LOOP ( 'NONE', ( #12827, #22155, #3883, #58 ) ) ;
#19576 = ORIENTED_EDGE ( 'NONE', *, *, #22769, .T. ) ;
#19577 = DIRECTION ( 'NONE',  ( -1.135604581876758782E-15, 1.065814103640148386E-14, 1.000000000000000000 ) ) ;
#19578 = EDGE_CURVE ( 'NONE', #9677, #15251, #4737, .T. ) ;
#19579 = EDGE_CURVE ( 'NONE', #18130, #12501, #8443, .T. ) ;
#19580 = FACE_OUTER_BOUND ( 'NONE', #2877, .T. ) ;
#19581 = DIRECTION ( 'NONE',  ( -1.129541670263356189E-15, -6.741645191078037727E-32, 1.000000000000000000 ) ) ;
#19582 = DIRECTION ( 'NONE',  ( 1.066788928082016908E-26, 3.471809175856251779E-58, -1.000000000000000000 ) ) ;
#19583 = CARTESIAN_POINT ( 'NONE',  ( -91.14322581977725690, -2.700000000000125855, 6.823838874241844543 ) ) ;
#19584 = DIRECTION ( 'NONE',  ( 1.000000000000000000, 6.224605580259554159E-31, -2.887593071917436153E-31 ) ) ;
#19585 = TOROIDAL_SURFACE ( 'NONE', #4549, 9.499999999999998224, 0.5000000000000000000 ) ;
#19586 = VECTOR ( 'NONE', #21015, 1000.000000000000114 ) ;
#19587 = DIRECTION ( 'NONE',  ( -2.168404344971008868E-16, 1.000000000000000000, 0.000000000000000000 ) ) ;
#19588 = DIRECTION ( 'NONE',  ( 1.000000000000000000, -4.440892098500654758E-16, 0.000000000000000000 ) ) ;
#19589 = SURFACE_SIDE_STYLE ('',( #14068 ) ) ;
#19590 = DIRECTION ( 'NONE',  ( 0.000000000000000000, 0.000000000000000000, 1.000000000000000000 ) ) ;
#19591 = DIRECTION ( 'NONE',  ( 3.254448077146059901E-32, 1.000000000000000000, 6.409494854920712161E-31 ) ) ;
#19592 = ADVANCED_FACE ( 'NONE', ( #19092 ), #15325, .T. ) ;
#19593 = EDGE_LOOP ( 'NONE', ( #14800, #9712, #4842, #6391 ) ) ;
#19594 = ADVANCED_FACE ( 'NONE', ( #12018 ), #1445, .F. ) ;
#19595 = ADVANCED_FACE ( 'NONE', ( #20640 ), #18984, .T. ) ;
#19596 = SURFACE_STYLE_FILL_AREA ( #8660 ) ;
#19597 = DIRECTION ( 'NONE',  ( 1.000000000000000000, -1.276756478318922725E-15, 1.333893503340766402E-15 ) ) ;
#19599 = VERTEX_POINT ( 'NONE', #7329 ) ;
#19598 = ORIENTED_EDGE ( 'NONE', *, *, #16659, .F. ) ;
#19600 =( REPRESENTATION_RELATIONSHIP ('NONE','NONE', #19450, #15574 ) REPRESENTATION_RELATIONSHIP_WITH_TRANSFORMATION ( #14822 )SHAPE_REPRESENTATION_RELATIONSHIP( ) );
#19601 = ORIENTED_EDGE ( 'NONE', *, *, #10968, .T. ) ;
#19602 = AXIS2_PLACEMENT_3D ( 'NONE', #17110, #1021, #15355 ) ;
#19603 = AXIS2_PLACEMENT_3D ( 'NONE', #6850, #8730, #20104 ) ;
#19605 = ORIENTED_EDGE ( 'NONE', *, *, #2470, .F. ) ;
#19604 = EDGE_CURVE ( 'NONE', #11001, #5105, #2028, .T. ) ;
#19606 = ORIENTED_EDGE ( 'NONE', *, *, #13816, .F. ) ;
#19607 = CARTESIAN_POINT ( 'NONE',  ( 124.5000000000018900, -6.500000000000061284, -6.500000000000040856 ) ) ;
#19608 = ADVANCED_FACE ( 'NONE', ( #10729 ), #19912, .F. ) ;
#19609 = CARTESIAN_POINT ( 'NONE',  ( -2.700000000000119194, 1.999999999999946265, -8.000000000000007105 ) ) ;
#19610 = CARTESIAN_POINT ( 'NONE',  ( 4.052424581287677796, 2.393186648133054373, -2.990837702970290835 ) ) ;
#19611 = EDGE_CURVE ( 'NONE', #19371, #17223, #9201, .T. ) ;
#19612 = DIRECTION ( 'NONE',  ( -5.551115123561405253E-17, -1.000000000000000000, -2.256980353643891447E-27 ) ) ;
#19613 = DIRECTION ( 'NONE',  ( 0.000000000000000000, -6.938893903907237844E-15, -1.000000000000000000 ) ) ;
#19614 = DIRECTION ( 'NONE',  ( -1.000000000000000000, 1.424116703980815236E-16, 2.931272055834072749E-32 ) ) ;
#19615 = CARTESIAN_POINT ( 'NONE',  ( 7.500000000000007105, -11.56013155386943758, 9.052558787159764364 ) ) ;
#19616 = CARTESIAN_POINT ( 'NONE',  ( 4.163336342344337027E-14, 3.469446951953614189E-14, -3.000000000000002665 ) ) ;
#19617 = CARTESIAN_POINT ( 'NONE',  ( 25.00000000000004619, 0.2499999999999863443, -1.999999999999998224 ) ) ;
#19618 = DIRECTION ( 'NONE',  ( -2.013525853228508439E-32, -6.779273404243028164E-31, 1.000000000000000000 ) ) ;
#19619 = VECTOR ( 'NONE', #11855, 1000.000000000000000 ) ;
#19620 = CARTESIAN_POINT ( 'NONE',  ( 0.000000000000000000, -1.750000000000001554, 0.000000000000000000 ) ) ;
#19621 = CARTESIAN_POINT ( 'NONE',  ( -42.54314575050793934, 5.299999999999998934, 7.500000000000062172 ) ) ;
#19622 = FACE_OUTER_BOUND ( 'NONE', #17103, .T. ) ;
#19623 = CIRCLE ( 'NONE', #18491, 4.500000000000031974 ) ;
#19624 = CARTESIAN_POINT ( 'NONE',  ( 0.000000000000000000, 3.031088913245528982, -1.750000000000001554 ) ) ;
#19625 = CARTESIAN_POINT ( 'NONE',  ( 3.973514160553476948, -3.435084588004225115, 1.181876024140334325 ) ) ;
#19626 = EDGE_LOOP ( 'NONE', ( #11111, #7486, #18670, #16999 ) ) ;
#19627 = AXIS2_PLACEMENT_3D ( 'NONE', #14272, #21685, #16244 ) ;
#19628 = ORIENTED_EDGE ( 'NONE', *, *, #3924, .F. ) ;
#19629 = ADVANCED_FACE ( 'NONE', ( #3337 ), #18579, .T. ) ;
#19630 = PLANE ( 'NONE',  #17018 ) ;
#19632 = ORIENTED_EDGE ( 'NONE', *, *, #1371, .T. ) ;
#19631 = ORIENTED_EDGE ( 'NONE', *, *, #3222, .T. ) ;
#19633 = VECTOR ( 'NONE', #10291, 1000.000000000000000 ) ;
#19634 = CARTESIAN_POINT ( 'NONE',  ( 119.5756419024615269, -4.500000000000003553, 6.500000000000123457 ) ) ;
#19635 = AXIS2_PLACEMENT_3D ( 'NONE', #19734, #1612, #7037 ) ;
#19636 = AXIS2_PLACEMENT_3D ( 'NONE', #17230, #905, #10176 ) ;
#19637 = CARTESIAN_POINT ( 'NONE',  ( 0.000000000000000000, 0.000000000000000000, -5.574599999999999334 ) ) ;
#19638 = EDGE_CURVE ( 'NONE', #4023, #1072, #16677, .T. ) ;
#19639 =( NAMED_UNIT ( * ) PLANE_ANGLE_UNIT ( ) SI_UNIT ( $, .RADIAN. ) );
#19640 = AXIS2_PLACEMENT_3D ( 'NONE', #6333, #806, #20919 ) ;
#19641 = FILL_AREA_STYLE_COLOUR ( '', #4853 ) ;
#19642 = ORIENTED_EDGE ( 'NONE', *, *, #15985, .F. ) ;
#19643 = LINE ( 'NONE', #6826, #13663 ) ;
#19644 = CARTESIAN_POINT ( 'NONE',  ( 1.199999999999992628, 6.996948694958265185E-16, -4.582731094065978894 ) ) ;
#19645 = LINE ( 'NONE', #7410, #20716 ) ;
#19646 = PRODUCT_DEFINITION_SHAPE ( 'NONE', 'NONE',  #22880 ) ;
#19647 = CARTESIAN_POINT ( 'NONE',  ( 0.6507732100473145875, -4.243078065514858999, -0.2236248678335386320 ) ) ;
#19648 = PLANE ( 'NONE',  #2814 ) ;
#19649 = CYLINDRICAL_SURFACE ( 'NONE', #5922, 0.4999999999999982236 ) ;
#19650 = DIRECTION ( 'NONE',  ( -2.220446049250313081E-16, 1.000000000000000000, -7.025792437124636392E-31 ) ) ;
#19651 = FACE_OUTER_BOUND ( 'NONE', #8090, .T. ) ;
#19652 = DIRECTION ( 'NONE',  ( -1.000000000000000000, -1.479114197289397135E-31, -5.916456789157588541E-31 ) ) ;
#19653 = AXIS2_PLACEMENT_3D ( 'NONE', #4766, #22897, #13604 ) ;
#19654 = AXIS2_PLACEMENT_3D ( 'NONE', #9660, #16703, #11193 ) ;
#19655 = CARTESIAN_POINT ( 'NONE',  ( 0.02944718078674108189, -0.6813962075909465455, 3.499999999999992895 ) ) ;
#19656 = CIRCLE ( 'NONE', #20023, 0.5000000000000038858 ) ;
#19657 = VERTEX_POINT ( 'NONE', #14268 ) ;
#19658 = TOROIDAL_SURFACE ( 'NONE', #4617, 5.500000000000000000, 0.5000000000000000000 ) ;
#19659 = EDGE_CURVE ( 'NONE', #1136, #10432, #14034, .T. ) ;
#19660 = SHAPE_DEFINITION_REPRESENTATION ( #1233, #16457 ) ;
#19662 = VERTEX_POINT ( 'NONE', #12484 ) ;
#19661 = ORIENTED_EDGE ( 'NONE', *, *, #9543, .F. ) ;
#19663 = ADVANCED_FACE ( 'NONE', ( #19555 ), #14452, .T. ) ;
#19664 = VERTEX_POINT ( 'NONE', #5216 ) ;
#19666 = ORIENTED_EDGE ( 'NONE', *, *, #17893, .F. ) ;
#19665 = ORIENTED_EDGE ( 'NONE', *, *, #21785, .F. ) ;
#19667 = CARTESIAN_POINT ( 'NONE',  ( -6.938893903907228378E-14, 4.999999999999976907, -4.163336342344337027E-14 ) ) ;
#19668 = EDGE_CURVE ( 'NONE', #17822, #10973, #4288, .T. ) ;
#19669 = DIRECTION ( 'NONE',  ( 0.000000000000000000, -1.000000000000000000, 0.000000000000000000 ) ) ;
#19670 = CARTESIAN_POINT ( 'NONE',  ( 7.024848138041158485, -11.34038014973665476, 8.468562630484207432 ) ) ;
#19671 = AXIS2_PLACEMENT_3D ( 'NONE', #21746, #677, #18550 ) ;
#19672 = FACE_OUTER_BOUND ( 'NONE', #3686, .T. ) ;
#19673 = AXIS2_PLACEMENT_3D ( 'NONE', #5297, #19530, #1869 ) ;
#19674 = FACE_OUTER_BOUND ( 'NONE', #8207, .T. ) ;
#19675 = AXIS2_PLACEMENT_3D ( 'NONE', #19527, #10699, #14341 ) ;
#19676 = CARTESIAN_POINT ( 'NONE',  ( -89.70000000000059970, 5.551115123125782702E-14, 1.000000000000000888 ) ) ;
#19677 = VECTOR ( 'NONE', #2068, 1000.000000000000000 ) ;
#19678 = CARTESIAN_POINT ( 'NONE',  ( 4.182403429330263656, -0.7499999999999387157, -2.876221860228560967 ) ) ;
#19679 = AXIS2_PLACEMENT_3D ( 'NONE', #13764, #4574, #4464 ) ;
#19680 = CIRCLE ( 'NONE', #525, 2.549999999999997158 ) ;
#19681 = DIRECTION ( 'NONE',  ( -1.454462294001240516E-30, -1.000000000000000000, -0.000000000000000000 ) ) ;
#19682 = CARTESIAN_POINT ( 'NONE',  ( -10.49999999999996803, -1.500000000000001332, 9.250000000000008882 ) ) ;
#19683 = CARTESIAN_POINT ( 'NONE',  ( 114.8016533820240852, -5.880524088665878502, -5.999999999999928946 ) ) ;
#19684 = DIRECTION ( 'NONE',  ( -1.000000000000000000, 4.190823558986610327E-31, -1.733449886265890494E-32 ) ) ;
#19685 = CARTESIAN_POINT ( 'NONE',  ( 2.775557561562891351E-14, 0.000000000000000000, -0.4999999999999865663 ) ) ;
#19686 = EDGE_CURVE ( 'NONE', #22849, #405, #12934, .T. ) ;
#19687 = DIRECTION ( 'NONE',  ( 0.5150787536377134934, 0.000000000000000000, -0.8571428571428567622 ) ) ;
#19688 = PLANE ( 'NONE',  #5175 ) ;
#19689 = CARTESIAN_POINT ( 'NONE',  ( -67.40537636629490237, -0.5000000000001045830, 12.70639812373640432 ) ) ;
#19690 = CARTESIAN_POINT ( 'NONE',  ( 3.950241966887844125, -3.393956070637585309, 1.121495646998712070 ) ) ;
#19691 = ORIENTED_EDGE ( 'NONE', *, *, #1110, .F. ) ;
#19692 = CIRCLE ( 'NONE', #2405, 0.5000000000000038858 ) ;
#19693 = FILL_AREA_STYLE ('',( #5338 ) ) ;
#19694 = VECTOR ( 'NONE', #9699, 1000.000000000000000 ) ;
#19696 = VERTEX_POINT ( 'NONE', #7211 ) ;
#19695 = VERTEX_POINT ( 'NONE', #2016 ) ;
#19697 = VECTOR ( 'NONE', #6540, 1000.000000000000000 ) ;
#19698 = ORIENTED_EDGE ( 'NONE', *, *, #208, .T. ) ;
#19700 = ORIENTED_EDGE ( 'NONE', *, *, #9642, .T. ) ;
#19699 = ORIENTED_EDGE ( 'NONE', *, *, #11105, .F. ) ;
#19701 = ORIENTED_EDGE ( 'NONE', *, *, #19412, .T. ) ;
#19702 = EDGE_LOOP ( 'NONE', ( #14129, #17512, #4774, #5468 ) ) ;
#19703 = ORIENTED_EDGE ( 'NONE', *, *, #4360, .F. ) ;
#19704 = ORIENTED_EDGE ( 'NONE', *, *, #16619, .F. ) ;
#19705 = PLANE ( 'NONE',  #2032 ) ;
#19706 = CARTESIAN_POINT ( 'NONE',  ( -50.65685424949275983, 7.200000000000018829, -8.000000000000007105 ) ) ;
#19707 = CARTESIAN_POINT ( 'NONE',  ( 113.0166151911346759, -11.64708151429785765, -6.500000000000040856 ) ) ;
#19708 = CARTESIAN_POINT ( 'NONE',  ( 86.02937988905580369, -9.453020409440155092, 6.500000000000165201 ) ) ;
#19709 = ADVANCED_FACE ( 'NONE', ( #5562 ), #3566, .F. ) ;
#19710 = AXIS2_PLACEMENT_3D ( 'NONE', #21097, #6739, #10379 ) ;
#19711 = CARTESIAN_POINT ( 'NONE',  ( 4.000000000000004441, -0.7779732554280850421, -5.566455648918319454 ) ) ;
#19712 = VECTOR ( 'NONE', #20631, 1000.000000000000000 ) ;
#19713 = CIRCLE ( 'NONE', #17831, 2.549999999999997158 ) ;
#19714 = CARTESIAN_POINT ( 'NONE',  ( -6.959810536856680940, 36.00015702695179698, -26.48940942388196618 ) ) ;
#19715 = DIRECTION ( 'NONE',  ( 3.791174248318675826E-31, 1.000000000000000000, 1.734723475976803347E-15 ) ) ;
#19716 = VECTOR ( 'NONE', #9924, 1000.000000000000000 ) ;
#19717 = LINE ( 'NONE', #19946, #11372 ) ;
#19718 = ADVANCED_FACE ( 'NONE', ( #8976 ), #21227, .F. ) ;
#19719 = SURFACE_STYLE_USAGE ( .BOTH. , #7142 ) ;
#19720 = LINE ( 'NONE', #6895, #9693 ) ;
#19721 = LINE ( 'NONE', #12175, #10275 ) ;
#19722 = CARTESIAN_POINT ( 'NONE',  ( -7.518994333257361440, -2.258039616118830750, 8.837702940568419763 ) ) ;
#19723 = AXIS2_PLACEMENT_3D ( 'NONE', #7474, #21827, #2285 ) ;
#19724 = EDGE_LOOP ( 'NONE', ( #9945, #8027, #314, #18162 ) ) ;
#19725 = EDGE_CURVE ( 'NONE', #3408, #22005, #6933, .T. ) ;
#19726 = PLANE ( 'NONE',  #730 ) ;
#19727 = FACE_OUTER_BOUND ( 'NONE', #22997, .T. ) ;
#19729 = ORIENTED_EDGE ( 'NONE', *, *, #745, .T. ) ;
#19728 = VERTEX_POINT ( 'NONE', #12607 ) ;
#19730 = ADVANCED_FACE ( 'NONE', ( #8736 ), #7681, .T. ) ;
#19731 = EDGE_LOOP ( 'NONE', ( #1939, #22501, #1608, #22039 ) ) ;
#19732 = VECTOR ( 'NONE', #1552, 1000.000000000000000 ) ;
#19733 = DIRECTION ( 'NONE',  ( -0.7313537016191730133, 0.6819983600624959230, -5.924440990721418971E-17 ) ) ;
#19734 = CARTESIAN_POINT ( 'NONE',  ( -55.25320565519140104, -3.200000000000108979, 10.00000000000007816 ) ) ;
#19735 = CARTESIAN_POINT ( 'NONE',  ( 73.50000000000115108, -6.999999999999811706, -6.938893903907228378E-15 ) ) ;
#19736 = CARTESIAN_POINT ( 'NONE',  ( -50.65685424949267457, -7.200000000000071232, -8.000000000000007105 ) ) ;
#19737 = EDGE_CURVE ( 'NONE', #6214, #6539, #3553, .T. ) ;
#19738 = ADVANCED_FACE ( 'NONE', ( #1683 ), #383, .F. ) ;
#19739 = CARTESIAN_POINT ( 'NONE',  ( 4.197393957002244491, 7.205051708611501750E-14, -3.503767560748914711 ) ) ;
#19740 = DIRECTION ( 'NONE',  ( -1.000000000000000000, -2.220446049250314067E-16, 5.825996348268307008E-33 ) ) ;
#19741 = DIRECTION ( 'NONE',  ( 1.000000000000000000, 2.891205793294682764E-16, 0.000000000000000000 ) ) ;
#19742 = DIRECTION ( 'NONE',  ( -5.551115123561405253E-17, -1.000000000000000000, -2.256980353643891447E-27 ) ) ;
#19743 = EDGE_CURVE ( 'NONE', #16151, #13355, #3187, .T. ) ;
#19744 = LINE ( 'NONE', #5275, #2824 ) ;
#19745 = CARTESIAN_POINT ( 'NONE',  ( 37.36637401601598185, 10.68627026436967675, -10.36637401601569231 ) ) ;
#19746 = CIRCLE ( 'NONE', #218, 6.000000000000047073 ) ;
#19747 = CARTESIAN_POINT ( 'NONE',  ( -47.47487373415324186, 4.018019484660552365, 8.000000000000062172 ) ) ;
#19748 = DIRECTION ( 'NONE',  ( -1.000000000000000000, 1.626303258728244079E-16, 0.000000000000000000 ) ) ;
#19749 = EDGE_CURVE ( 'NONE', #5108, #19664, #16301, .T. ) ;
#19750 = EDGE_CURVE ( 'NONE', #8991, #8999, #22130, .T. ) ;
#19751 = DIRECTION ( 'NONE',  ( -1.000000000000000000, -2.699383410053119644E-30, -3.330669073875432643E-16 ) ) ;
#19752 = CARTESIAN_POINT ( 'NONE',  ( 3.999999999999955147, -3.469446951953614189E-14, 0.000000000000000000 ) ) ;
#19753 = ORIENTED_EDGE ( 'NONE', *, *, #20349, .F. ) ;
#19754 = EDGE_LOOP ( 'NONE', ( #718, #23266, #805, #3304 ) ) ;
#19755 = CARTESIAN_POINT ( 'NONE',  ( 5.600000000000000533, 0.000000000000000000, -3.469446951953614189E-15 ) ) ;
#19756 = ORIENTED_EDGE ( 'NONE', *, *, #15823, .F. ) ;
#19757 = DIRECTION ( 'NONE',  ( -1.725633230170960916E-31, -1.000000000000000000, -2.220446049250310616E-16 ) ) ;
#19758 = DIRECTION ( 'NONE',  ( -1.000000000000000000, 1.276756478318922922E-15, 1.333893503340774882E-15 ) ) ;
#19759 = ADVANCED_FACE ( 'NONE', ( #12839 ), #14839, .F. ) ;
#19760 = CARTESIAN_POINT ( 'NONE',  ( 8.079084010241055935, -11.97965595983265352, 6.665520415301795509 ) ) ;
#19761 = FILL_AREA_STYLE ('',( #19641 ) ) ;
#19762 = EDGE_CURVE ( 'NONE', #13382, #22677, #14823, .T. ) ;
#19763 = ORIENTED_EDGE ( 'NONE', *, *, #19659, .T. ) ;
#19764 = AXIS2_PLACEMENT_3D ( 'NONE', #1336, #17309, #19323 ) ;
#19765 = DIRECTION ( 'NONE',  ( 1.000000000000000000, 4.252453317207022894E-31, -5.551115123125818447E-17 ) ) ;
#19766 = CARTESIAN_POINT ( 'NONE',  ( -0.4634555468559507507, -1.749999999999993561, -4.750000000000024869 ) ) ;
#19767 = DIRECTION ( 'NONE',  ( 1.000000000000000000, -4.437342591868175641E-31, 3.330669073875457788E-16 ) ) ;
#19768 = CARTESIAN_POINT ( 'NONE',  ( -8.697224362268011433, -14.00000000000004441, 6.250000000000033751 ) ) ;
#19769 = DIRECTION ( 'NONE',  ( -1.550910762415566494E-16, -1.000000000000000000, 8.135128085091684243E-31 ) ) ;
#19770 = CARTESIAN_POINT ( 'NONE',  ( 8.165409815605466193, -2.008174044758946231, 6.581206704444427125 ) ) ;
#19771 = B_SPLINE_CURVE_WITH_KNOTS ( 'NONE', 3,
 ( #3364, #19113, #19227, #10524, #17690, #3467 ),
 .UNSPECIFIED., .F., .F.,
 ( 4, 2, 4 ),
 ( 0.003805860999069573050, 0.004828937044845143384, 0.005852013090620712850 ),
 .UNSPECIFIED. ) ;
#19772 = CARTESIAN_POINT ( 'NONE',  ( 4.114405500665263560, 2.025575754679722618, -3.508400121684928319 ) ) ;
#19773 = CARTESIAN_POINT ( 'NONE',  ( 3.948103430091023380, -2.682758828852069843, 2.353325403973813401 ) ) ;
#19774 = ADVANCED_FACE ( 'NONE', ( #18376 ), #5901, .T. ) ;
#19775 = CARTESIAN_POINT ( 'NONE',  ( -3.997250504095343437, 1.750000000000008882, 2.576559036326544483 ) ) ;
#19776 = CARTESIAN_POINT ( 'NONE',  ( 3.999999999999938716, 0.7924765000094652345, -0.05906175389885159194 ) ) ;
#19777 = ORIENTED_EDGE ( 'NONE', *, *, #4454, .F. ) ;
#19778 = ITEM_DEFINED_TRANSFORMATION ( 'NONE', 'NONE', #3002,  #22115 ) ;
#19780 = VERTEX_POINT ( 'NONE', #2126 ) ;
#19779 = ORIENTED_EDGE ( 'NONE', *, *, #21745, .T. ) ;
#19781 = CIRCLE ( 'NONE', #19398, 4.249999999999965361 ) ;
#19782 = VERTEX_POINT ( 'NONE', #11299 ) ;
#19784 = ORIENTED_EDGE ( 'NONE', *, *, #18439, .T. ) ;
#19783 = EDGE_LOOP ( 'NONE', ( #22150, #15851, #13758, #9135 ) ) ;
#19785 = CARTESIAN_POINT ( 'NONE',  ( 0.5636800770122561977, 4.293361309316750862, -3.531542292954451767 ) ) ;
#19786 = CARTESIAN_POINT ( 'NONE',  ( -3.999999999708153453, 42.99999999900385461, -18.50000000000000355 ) ) ;
#19787 = CARTESIAN_POINT ( 'NONE',  ( 7.854293383767760872, -11.68772904158814008, 7.820081954006964153 ) ) ;
#19788 = CARTESIAN_POINT ( 'NONE',  ( -7.576750937466543157, -11.88724926130080028, 7.200086239788027420 ) ) ;
#19789 = DIRECTION ( 'NONE',  ( 0.000000000000000000, 0.000000000000000000, -1.000000000000000000 ) ) ;
#19790 = CARTESIAN_POINT ( 'NONE',  ( 24.75000000000001776, 0.2500000000000418554, -2.000000000000022649 ) ) ;
#19791 = ADVANCED_FACE ( 'NONE', ( #2363 ), #925, .T. ) ;
#19792 = DIRECTION ( 'NONE',  ( -1.066786462891689527E-26, -6.656013887802287108E-31, -1.000000000000000000 ) ) ;
#19793 = CARTESIAN_POINT ( 'NONE',  ( 0.000000000000000000, 0.000000000000000000, -5.000000000000000888 ) ) ;
#19794 = AXIS2_PLACEMENT_3D ( 'NONE', #17019, #11854, #9983 ) ;
#19795 = CARTESIAN_POINT ( 'NONE',  ( 6.999999999999978684, -3.018576030000261312, 8.916666666666724694 ) ) ;
#19796 = LINE ( 'NONE', #23108, #6178 ) ;
#19797 = CARTESIAN_POINT ( 'NONE',  ( 5.035458327682277080, -1.561572887838371226, -0.7783303370585006320 ) ) ;
#19798 = ADVANCED_FACE ( 'NONE', ( #20494 ), #14609, .T. ) ;
#19799 = AXIS2_PLACEMENT_3D ( 'NONE', #739, #20505, #11427 ) ;
#19800 = CARTESIAN_POINT ( 'NONE',  ( 4.578118944855308570, 1.701165921963294858, 1.570465384416993349 ) ) ;
#19801 = FACE_OUTER_BOUND ( 'NONE', #10456, .T. ) ;
#19802 = CARTESIAN_POINT ( 'NONE',  ( -47.47487373415321343, -4.018019484660608320, -7.500000000000007105 ) ) ;
#19803 = FACE_OUTER_BOUND ( 'NONE', #19220, .T. ) ;
#19804 = ADVANCED_FACE ( 'NONE', ( #5800 ), #12961, .T. ) ;
#19805 = EDGE_LOOP ( 'NONE', ( #20915, #6528, #2533, #18292 ) ) ;
#19807 = EDGE_LOOP ( 'NONE', ( #11814, #6588, #12713 ) ) ;
#19806 = ORIENTED_EDGE ( 'NONE', *, *, #4175, .F. ) ;
#19808 = ORIENTED_EDGE ( 'NONE', *, *, #10402, .T. ) ;
#19810 = ORIENTED_EDGE ( 'NONE', *, *, #18170, .F. ) ;
#19809 = ORIENTED_EDGE ( 'NONE', *, *, #14851, .T. ) ;
#19811 = VERTEX_POINT ( 'NONE', #6373 ) ;
#19812 = AXIS2_PLACEMENT_3D ( 'NONE', #2206, #6209, #21024 ) ;
#19813 = VERTEX_POINT ( 'NONE', #18957 ) ;
#19814 = EDGE_LOOP ( 'NONE', ( #5704, #8607, #10623, #9505 ) ) ;
#19815 = CARTESIAN_POINT ( 'NONE',  ( -50.65685424949274562, 7.200000000000025935, 17.71251237973613257 ) ) ;
#19816 = AXIS2_PLACEMENT_3D ( 'NONE', #11887, #4590, #22960 ) ;
#19817 = PRESENTATION_STYLE_ASSIGNMENT (( #2043 ) ) ;
#19818 = CARTESIAN_POINT ( 'NONE',  ( 58.85734743794746038, 0.7537990605245292741, 6.500000000000123457 ) ) ;
#19819 = PLANE ( 'NONE',  #13629 ) ;
#19820 = CIRCLE ( 'NONE', #18359, 4.750000000000000000 ) ;
#19821 = CARTESIAN_POINT ( 'NONE',  ( 4.104070371397483541, -2.023683613428375772, -3.505122836902536232 ) ) ;
#19822 = DIRECTION ( 'NONE',  ( 0.000000000000000000, -1.000000000000000000, 0.000000000000000000 ) ) ;
#19823 = CARTESIAN_POINT ( 'NONE',  ( -1.390230914382294847, -4.043987460488769337, -3.502507215260536988 ) ) ;
#19824 = FILL_AREA_STYLE ('',( #10643 ) ) ;
#19825 = VECTOR ( 'NONE', #13462, 1000.000000000000000 ) ;
#19826 = CARTESIAN_POINT ( 'NONE',  ( -2.700000000000091216, -2.000000000000001776, -7.500000000000034639 ) ) ;
#19827 = CARTESIAN_POINT ( 'NONE',  ( 0.000000000000000000, 0.000000000000000000, 0.000000000000000000 ) ) ;
#19828 = VECTOR ( 'NONE', #15617, 1000.000000000000000 ) ;
#19829 = DIRECTION ( 'NONE',  ( -1.686884416050044188E-17, 0.9863939238321436376, 0.1643989873053578188 ) ) ;
#19830 = CIRCLE ( 'NONE', #7438, 4.000000000000000000 ) ;
#19831 = ORIENTED_EDGE ( 'NONE', *, *, #2034, .T. ) ;
#19832 = SURFACE_STYLE_USAGE ( .BOTH. , #12413 ) ;
#19833 = LINE ( 'NONE', #15818, #18375 ) ;
#19835 = EDGE_LOOP ( 'NONE', ( #2825, #123, #20304, #7683 ) ) ;
#19834 = EDGE_LOOP ( 'NONE', ( #7262, #2215, #19030, #8841 ) ) ;
#19836 = CIRCLE ( 'NONE', #9689, 0.4999999999999995559 ) ;
#19837 = VECTOR ( 'NONE', #7336, 1000.000000000000000 ) ;
#19838 = VERTEX_POINT ( 'NONE', #8013 ) ;
#19839 = ORIENTED_EDGE ( 'NONE', *, *, #19941, .F. ) ;
#19840 = ORIENTED_EDGE ( 'NONE', *, *, #5927, .T. ) ;
#19841 = ADVANCED_FACE ( 'NONE', ( #15641 ), #6600, .T. ) ;
#19842 = CARTESIAN_POINT ( 'NONE',  ( 88.75737332930587797, -11.02760560296348125, 6.500000000000075495 ) ) ;
#19843 = CARTESIAN_POINT ( 'NONE',  ( 33.59619407800441593, 21.59619407671642222, -19.00000000000000355 ) ) ;
#19844 = CARTESIAN_POINT ( 'NONE',  ( 4.175813232069149450, -2.061359961916378492, -3.570380186727402538 ) ) ;
#19845 = CIRCLE ( 'NONE', #9706, 0.5000000000000017764 ) ;
#19846 = CARTESIAN_POINT ( 'NONE',  ( 37.50000000000016342, -2.613291509943991698E-15, -10.68301270189226848 ) ) ;
#19847 = CARTESIAN_POINT ( 'NONE',  ( -43.46238456605044576, -4.919238815542552601, 8.000000000000035527 ) ) ;
#19848 = DIRECTION ( 'NONE',  ( -3.254448077146059901E-32, -1.000000000000000000, -6.409494854920712161E-31 ) ) ;
#19849 = CARTESIAN_POINT ( 'NONE',  ( -55.25320565519150051, 0.5000000000000905942, 7.500000000000062172 ) ) ;
#19850 = DIRECTION ( 'NONE',  ( 0.7071067811865495711, -0.7071067811865455743, -4.556821512286142627E-17 ) ) ;
#19851 = DIRECTION ( 'NONE',  ( 3.885780586188016830E-16, 4.437342591868156373E-31, -1.000000000000000000 ) ) ;
#19852 = VECTOR ( 'NONE', #7192, 1000.000000000000000 ) ;
#19853 = CARTESIAN_POINT ( 'NONE',  ( 3.000000000291852764, 42.99999999900385461, -25.50000000000000355 ) ) ;
#19854 = B_SPLINE_CURVE_WITH_KNOTS ( 'NONE', 3,
 ( #1592, #1930, #9119, #23258 ),
 .UNSPECIFIED., .F., .F.,
 ( 4, 4 ),
 ( 2.380739283250810230E-07, 0.002044882221487500686 ),
 .UNSPECIFIED. ) ;
#19855 = AXIS2_PLACEMENT_3D ( 'NONE', #17525, #13890, #21074 ) ;
#19856 = CIRCLE ( 'NONE', #330, 4.500000000000045297 ) ;
#19857 = CARTESIAN_POINT ( 'NONE',  ( 8.495599073428120818, -1.515757017040944898, 7.013360899078348254 ) ) ;
#19858 = CARTESIAN_POINT ( 'NONE',  ( 12.49999999999995914, 2.775557561562891982E-14, -14.50000000000000355 ) ) ;
#19859 = CARTESIAN_POINT ( 'NONE',  ( -6.495190528383341544, 4.999999999999920952, 3.750000000000017319 ) ) ;
#19860 = CARTESIAN_POINT ( 'NONE',  ( 10.50000000000000888, -13.50000000000003020, 5.750000000000060396 ) ) ;
#19861 = CARTESIAN_POINT ( 'NONE',  ( 4.175813232069142344, -2.061359961916364725, 3.570380186727402538 ) ) ;
#19862 = VERTEX_POINT ( 'NONE', #17169 ) ;
#19863 = ADVANCED_FACE ( 'NONE', ( #6717 ), #8359, .F. ) ;
#19864 = ORIENTED_EDGE ( 'NONE', *, *, #17121, .T. ) ;
#19865 = CIRCLE ( 'NONE', #1825, 5.000000000000000888 ) ;
#19866 = ADVANCED_FACE ( 'NONE', ( #22372 ), #18966, .T. ) ;
#19867 = DIRECTION ( 'NONE',  ( 0.9706398123736329486, -1.505375731439247187E-16, 0.2405376366294442458 ) ) ;
#19868 = AXIS2_PLACEMENT_3D ( 'NONE', #8340, #6351, #13525 ) ;
#19869 = DIRECTION ( 'NONE',  ( -0.7313537016191735685, 0.6819983600624951459, -3.923113172947598083E-16 ) ) ;
#19870 = VERTEX_POINT ( 'NONE', #1314 ) ;
#19871 = DIRECTION ( 'NONE',  ( -1.066723072283234472E-26, 0.000000000000000000, -1.000000000000000000 ) ) ;
#19872 = CARTESIAN_POINT ( 'NONE',  ( -10.49999999999995381, -2.000000000000005329, 9.249999999999966249 ) ) ;
#19873 = CARTESIAN_POINT ( 'NONE',  ( 3.948103430091032706, -3.379418997639192401, -1.146674596025634152 ) ) ;
#19874 = CARTESIAN_POINT ( 'NONE',  ( 0.3126073911696378160, 2.020725942163612121, 3.499999999999975131 ) ) ;
#19876 = ORIENTED_EDGE ( 'NONE', *, *, #1496, .T. ) ;
#19875 = ADVANCED_FACE ( 'NONE', ( #15293 ), #15525, .F. ) ;
#19877 = CARTESIAN_POINT ( 'NONE',  ( 3.973110223767139626, 2.264800795684280898E-11, 3.565797985667429781 ) ) ;
#19878 = LINE ( 'NONE', #10472, #14196 ) ;
#19879 = EDGE_CURVE ( 'NONE', #10484, #16918, #942, .T. ) ;
#19880 = APPLICATION_CONTEXT ( 'automotive_design' ) ;
#19881 = CARTESIAN_POINT ( 'NONE',  ( 6.000000000291855429, 2.999999999003851503, -39.00000000000000000 ) ) ;
#19882 = EDGE_CURVE ( 'NONE', #477, #19955, #7334, .T. ) ;
#19883 = CARTESIAN_POINT ( 'NONE',  ( 4.071447262713884463, 2.020725942163681399, 3.499999999999996003 ) ) ;
#19884 = COLOUR_RGB ( '', 0.72549020, 0.75294118, 0.79215686) ;
#19885 = CARTESIAN_POINT ( 'NONE',  ( 7.499999999999978684, -12.60977222864647196, 9.250000000000087041 ) ) ;
#19886 = CARTESIAN_POINT ( 'NONE',  ( -50.65685424949280247, 1.387778780781445676E-14, 8.000000000000090594 ) ) ;
#19887 = LINE ( 'NONE', #12347, #17981 ) ;
#19888 =( LENGTH_UNIT ( ) NAMED_UNIT ( * ) SI_UNIT ( .MILLI., .METRE. ) );
#19889 = CIRCLE ( 'NONE', #4088, 3.500000000000004441 ) ;
#19890 = DIRECTION ( 'NONE',  ( 1.550910762415566494E-16, 1.000000000000000000, -8.135128085091684243E-31 ) ) ;
#19891 = ADVANCED_FACE ( 'NONE', ( #2706 ), #1085, .F. ) ;
#19892 = EDGE_LOOP ( 'NONE', ( #3211, #7196, #16027 ) ) ;
#19893 = EDGE_CURVE ( 'NONE', #23148, #17301, #13888, .T. ) ;
#19894 = EDGE_CURVE ( 'NONE', #8929, #22821, #20723, .T. ) ;
#19895 = SHAPE_DEFINITION_REPRESENTATION ( #22833, #4297 ) ;
#19896 = AXIS2_PLACEMENT_3D ( 'NONE', #4095, #19011, #11826 ) ;
#19898 = VERTEX_POINT ( 'NONE', #4715 ) ;
#19897 = ORIENTED_EDGE ( 'NONE', *, *, #23225, .T. ) ;
#19899 =( GEOMETRIC_REPRESENTATION_CONTEXT ( 3 ) GLOBAL_UNCERTAINTY_ASSIGNED_CONTEXT ( ( #19950 ) ) GLOBAL_UNIT_ASSIGNED_CONTEXT ( ( #14852, #11082, #7452 ) ) REPRESENTATION_CONTEXT ( 'NONE', 'WORKASPACE' ) );
#19900 = VERTEX_POINT ( 'NONE', #20956 ) ;
#19902 = ORIENTED_EDGE ( 'NONE', *, *, #20442, .F. ) ;
#19901 = ORIENTED_EDGE ( 'NONE', *, *, #17854, .F. ) ;
#19903 = EDGE_CURVE ( 'NONE', #16918, #13467, #13112, .T. ) ;
#19904 = CARTESIAN_POINT ( 'NONE',  ( 3.453038570459371570, 2.625189405339196647, -3.535263753544082288 ) ) ;
#19905 = CARTESIAN_POINT ( 'NONE',  ( 7.473326079327783589, -0.1514770120355188321, 7.598194856234280259 ) ) ;
#19906 = CARTESIAN_POINT ( 'NONE',  ( 7.802869476033197138, -11.64353246333685021, 7.917139222843311508 ) ) ;
#19907 = EDGE_CURVE ( 'NONE', #14175, #22294, #14467, .T. ) ;
#19908 = FACE_OUTER_BOUND ( 'NONE', #7914, .T. ) ;
#19909 = LINE ( 'NONE', #17911, #12781 ) ;
#19910 = CARTESIAN_POINT ( 'NONE',  ( 2.918498775983380256E-10, 5.999999999003851059, -29.00000000000000355 ) ) ;
#19911 = DIRECTION ( 'NONE',  ( -1.000000000000000000, 1.550910762415566494E-16, -8.566929763922626680E-48 ) ) ;
#19912 = CYLINDRICAL_SURFACE ( 'NONE', #4670, 2.800000000000017142 ) ;
#19913 = DIRECTION ( 'NONE',  ( 1.333893503340774882E-15, 2.778352770573747380E-17, 1.000000000000000000 ) ) ;
#19914 = AXIS2_PLACEMENT_3D ( 'NONE', #14866, #9459, #5474 ) ;
#19915 = CARTESIAN_POINT ( 'NONE',  ( 54.42435809754115894, -8.326672684688674053E-14, -5.999999999999950262 ) ) ;
#19916 = APPLICATION_CONTEXT ( 'automotive_design' ) ;
#19917 = CARTESIAN_POINT ( 'NONE',  ( 4.630153689607049650, 0.000000000000000000, 0.000000000000000000 ) ) ;
#19918 = AXIS2_PLACEMENT_3D ( 'NONE', #4724, #2967, #7905 ) ;
#19919 = DIRECTION ( 'NONE',  ( -2.013525853228518840E-32, 6.902532920683810383E-31, -1.000000000000000000 ) ) ;
#19920 = CARTESIAN_POINT ( 'NONE',  ( -10.49999999999995381, -1.499999999999997780, 6.250000000000019540 ) ) ;
#19921 = CARTESIAN_POINT ( 'NONE',  ( 0.3126073911696447549, 2.020725942163688504, -3.499999999999996003 ) ) ;
#19922 = CYLINDRICAL_SURFACE ( 'NONE', #20554, 0.5000000000000037748 ) ;
#19923 = ORIENTED_EDGE ( 'NONE', *, *, #5106, .F. ) ;
#19924 = SURFACE_STYLE_USAGE ( .BOTH. , #12738 ) ;
#19926 = ORIENTED_EDGE ( 'NONE', *, *, #14362, .T. ) ;
#19925 = VERTEX_POINT ( 'NONE', #15179 ) ;
#19927 = UNCERTAINTY_MEASURE_WITH_UNIT (LENGTH_MEASURE( 1.000000000000000082E-05 ), #16888, 'distance_accuracy_value', 'NONE');
#19928 = ORIENTED_EDGE ( 'NONE', *, *, #1783, .T. ) ;
#19930 = VERTEX_POINT ( 'NONE', #11994 ) ;
#19929 = ORIENTED_EDGE ( 'NONE', *, *, #12539, .F. ) ;
#19931 = AXIS2_PLACEMENT_3D ( 'NONE', #2858, #17198, #869 ) ;
#19932 = ORIENTED_EDGE ( 'NONE', *, *, #6970, .F. ) ;
#19933 = EDGE_CURVE ( 'NONE', #2382, #14190, #20991, .T. ) ;
#19934 = CARTESIAN_POINT ( 'NONE',  ( -12.85000000000001386, -14.00000000000007105, 5.551115123125782702E-14 ) ) ;
#19935 = EDGE_CURVE ( 'NONE', #5552, #7007, #6645, .T. ) ;
#19936 = ORIENTED_EDGE ( 'NONE', *, *, #13389, .F. ) ;
#19937 = VERTEX_POINT ( 'NONE', #10231 ) ;
#19938 = CARTESIAN_POINT ( 'NONE',  ( 110.9706201109471522, -11.02760560296359138, 6.500000000000095923 ) ) ;
#19939 = DIRECTION ( 'NONE',  ( 0.7071067811865268116, -0.7071067811865682229, -1.010793663541205907E-16 ) ) ;
#19940 = CARTESIAN_POINT ( 'NONE',  ( -95.70000000000058549, -1.318389841742373392E-13, 1.000000000000014655 ) ) ;
#19941 = EDGE_CURVE ( 'NONE', #12862, #1669, #22485, .T. ) ;
#19942 = LINE ( 'NONE', #187, #1600 ) ;
#19943 = DIRECTION ( 'NONE',  ( 0.7071067811865485719, -0.7071067811865464625, -1.010793663541191362E-16 ) ) ;
#19944 = DIRECTION ( 'NONE',  ( -2.172745813409349776E-17, 1.000000000000000000, -1.309377075419428048E-16 ) ) ;
#19945 = CARTESIAN_POINT ( 'NONE',  ( -0.5449313310647870834, -4.304185902836999311, -3.316620875263376789 ) ) ;
#19946 = CARTESIAN_POINT ( 'NONE',  ( -66.55000000000046612, 6.188383139260622304E-14, -1.999999999999974021 ) ) ;
#19947 = FACE_OUTER_BOUND ( 'NONE', #22770, .T. ) ;
#19948 = DIRECTION ( 'NONE',  ( 0.000000000000000000, 0.000000000000000000, 1.000000000000000000 ) ) ;
#19949 = EDGE_LOOP ( 'NONE', ( #8415, #2966, #3318, #4056 ) ) ;
#19950 = UNCERTAINTY_MEASURE_WITH_UNIT (LENGTH_MEASURE( 1.000000000000000082E-05 ), #14852, 'distance_accuracy_value', 'NONE');
#19951 =( NAMED_UNIT ( * ) PLANE_ANGLE_UNIT ( ) SI_UNIT ( $, .RADIAN. ) );
#19953 = ORIENTED_EDGE ( 'NONE', *, *, #10256, .T. ) ;
#19952 = ORIENTED_EDGE ( 'NONE', *, *, #15288, .T. ) ;
#19954 = ORIENTED_EDGE ( 'NONE', *, *, #16401, .T. ) ;
#19955 = VERTEX_POINT ( 'NONE', #6961 ) ;
#19956 = ORIENTED_EDGE ( 'NONE', *, *, #12959, .F. ) ;
#19957 = FACE_OUTER_BOUND ( 'NONE', #5200, .T. ) ;
#19958 = AXIS2_PLACEMENT_3D ( 'NONE', #9145, #16071, #16310 ) ;
#19959 = AXIS2_PLACEMENT_3D ( 'NONE', #2893, #10073, #6318 ) ;
#19960 = DIRECTION ( 'NONE',  ( -1.000000000000000000, 1.276756478318923119E-15, -1.239088197126283964E-15 ) ) ;
#19961 = CARTESIAN_POINT ( 'NONE',  ( 4.071447262713884463, -2.020725942163695166, -3.500000000000000444 ) ) ;
#19962 = CARTESIAN_POINT ( 'NONE',  ( 2.775557561562891351E-14, 0.5000000000000004441, -2.133974596215532316 ) ) ;
#19963 = DIRECTION ( 'NONE',  ( 1.454462294001240516E-30, 1.000000000000000000, 0.000000000000000000 ) ) ;
#19964 = CARTESIAN_POINT ( 'NONE',  ( 12.84999999999997300, -0.5000000000000004441, -5.749999999999963585 ) ) ;
#19965 = DIRECTION ( 'NONE',  ( -1.134196829589822059E-15, -6.741645191078037727E-32, 1.000000000000000000 ) ) ;
#19966 = CARTESIAN_POINT ( 'NONE',  ( -8.565230440156010872, -1.999999999999984457, 6.320505311736922316 ) ) ;
#19967 = CARTESIAN_POINT ( 'NONE',  ( 37.86602540378474657, 11.00000000000000533, -10.86602540378446591 ) ) ;
#19968 = CARTESIAN_POINT ( 'NONE',  ( 8.391189084741263571, -1.526797151860789903, 7.111621047081309044 ) ) ;
#19969 = CARTESIAN_POINT ( 'NONE',  ( -45.37157287525418781, 6.828427124746204058, -7.500000000000007105 ) ) ;
#19970 = DIRECTION ( 'NONE',  ( 1.000000000000000000, 0.000000000000000000, 0.000000000000000000 ) ) ;
#19971 = EDGE_CURVE ( 'NONE', #4498, #15879, #5790, .T. ) ;
#19972 = CYLINDRICAL_SURFACE ( 'NONE', #8975, 4.750000000000000000 ) ;
#19973 = TOROIDAL_SURFACE ( 'NONE', #19602, 2.500000000000003997, 0.5000000000000000000 ) ;
#19974 = AXIS2_PLACEMENT_3D ( 'NONE', #9282, #15888, #12132 ) ;
#19975 = B_SPLINE_CURVE_WITH_KNOTS ( 'NONE', 3,
 ( #3422, #14472, #8831, #9052, #17643, #16212, #12460, #1535, #12219, #23076, #14239, #1760, #6960, #19768 ),
 .UNSPECIFIED., .F., .F.,
 ( 4, 2, 2, 2, 2, 2, 4 ),
 ( 0.000000000000000000, 0.001000930383652479713, 0.001501395575478720870, 0.002001860767304962027, 0.002502325959131202968, 0.003002791150957444342, 0.004003721534609925789 ),
 .UNSPECIFIED. ) ;
#19976 = ORIENTED_EDGE ( 'NONE', *, *, #9386, .T. ) ;
#19977 = ORIENTED_EDGE ( 'NONE', *, *, #3523, .T. ) ;
#19978 = DIRECTION ( 'NONE',  ( -1.000000000000000000, 1.389842848855773367E-62, -2.013525853228507892E-32 ) ) ;
#19979 = CARTESIAN_POINT ( 'NONE',  ( 37.00000000000014211, 11.00000000000000000, -3.000000000000002665 ) ) ;
#19980 = EDGE_LOOP ( 'NONE', ( #3794, #4222, #22588, #780 ) ) ;
#19981 = DIRECTION ( 'NONE',  ( -5.004010026856173173E-16, -1.201780285297635391E-31, 1.000000000000000000 ) ) ;
#19982 = DIRECTION ( 'NONE',  ( 0.8660254037844387076, 1.577721810442023611E-30, 0.5000000000000001110 ) ) ;
#19983 = CARTESIAN_POINT ( 'NONE',  ( 3.961551342853102398, -2.319461885623262276, -2.982574167881092642 ) ) ;
#19984 = DIRECTION ( 'NONE',  ( 0.000000000000000000, -3.382522293539642133E-32, -1.000000000000000000 ) ) ;
#19985 = ORIENTED_EDGE ( 'NONE', *, *, #4722, .F. ) ;
#19986 = DIRECTION ( 'NONE',  ( -1.000000000000000000, -3.254448077276381206E-32, -1.066788928082016908E-26 ) ) ;
#19987 = AXIS2_PLACEMENT_3D ( 'NONE', #20366, #6137, #18606 ) ;
#19988 = LINE ( 'NONE', #22105, #7063 ) ;
#19989 = DIRECTION ( 'NONE',  ( 0.000000000000000000, 0.000000000000000000, -1.000000000000000000 ) ) ;
#19990 = CARTESIAN_POINT ( 'NONE',  ( 8.414481090081482151, -14.00000000000005151, 6.435353702847478985 ) ) ;
#19991 = CARTESIAN_POINT ( 'NONE',  ( -6.000000000000130562, 1.999999999999960032, -8.000000000000035527 ) ) ;
#19992 = LINE ( 'NONE', #5655, #23217 ) ;
#19993 = CARTESIAN_POINT ( 'NONE',  ( 4.086376042167607636, 1.979461949354216932, -3.571471332069190652 ) ) ;
#19994 = CARTESIAN_POINT ( 'NONE',  ( 37.86602540378461157, 11.00000000000000000, -6.500000000000005329 ) ) ;
#19995 = LINE ( 'NONE', #5886, #1405 ) ;
#19996 = ADVANCED_FACE ( 'NONE', ( #7077 ), #23077, .F. ) ;
#19997 = STYLED_ITEM ( 'NONE', ( #11567 ), #5304 ) ;
#19998 = CARTESIAN_POINT ( 'NONE',  ( 3.999999999999940936, 2.309401076758546445, -0.5000000000000004441 ) ) ;
#19999 = EDGE_CURVE ( 'NONE', #20601, #8098, #21974, .T. ) ;
#20000 = APPLICATION_PROTOCOL_DEFINITION ( 'draft international standard', 'automotive_design', 1998, #3529 ) ;
#20001 = AXIS2_PLACEMENT_3D ( 'NONE', #22622, #10264, #8503 ) ;
#20002 = EDGE_CURVE ( 'NONE', #19565, #11343, #5059, .T. ) ;
#20003 = ORIENTED_EDGE ( 'NONE', *, *, #4641, .F. ) ;
#20004 = CONICAL_SURFACE ( 'NONE', #20777, 3.500000000000004441, 1.047197551196600296 ) ;
#20005 = EDGE_CURVE ( 'NONE', #18914, #11721, #3423, .T. ) ;
#20006 = VECTOR ( 'NONE', #16068, 1000.000000000000000 ) ;
#20007 = VERTEX_POINT ( 'NONE', #1870 ) ;
#20008 = AXIS2_PLACEMENT_3D ( 'NONE', #11724, #19033, #16773 ) ;
#20010 = EDGE_LOOP ( 'NONE', ( #4160, #3795, #8903, #16635, #2065, #13187 ) ) ;
#20009 = ORIENTED_EDGE ( 'NONE', *, *, #7529, .T. ) ;
#20011 = DIRECTION ( 'NONE',  ( -3.241725282392603095E-30, -1.000000000000000000, 2.218671295934100958E-31 ) ) ;
#20012 = CARTESIAN_POINT ( 'NONE',  ( 7.000000000000007105, -0.7870719649792512485, 9.239863038076343571 ) ) ;
#20013 = CARTESIAN_POINT ( 'NONE',  ( 7.568091547084029536, -11.30436690654924803, 8.516664522246443880 ) ) ;
#20014 = DIRECTION ( 'NONE',  ( -9.121204216617949000E-31, -1.000000000000000000, 6.982962677686261977E-15 ) ) ;
#20015 = B_SPLINE_CURVE_WITH_KNOTS ( 'NONE', 3,
 ( #15611, #4684, #13960, #23036, #19038, #1049 ),
 .UNSPECIFIED., .F., .F.,
 ( 4, 2, 4 ),
 ( 0.002044882221487581784, 0.003063384235218523204, 0.004081886248949465057 ),
 .UNSPECIFIED. ) ;
#20016 = LINE ( 'NONE', #3892, #7896 ) ;
#20017 = DIRECTION ( 'NONE',  ( -3.070652698126927723E-17, -1.000000000000000000, 4.167305704548413124E-17 ) ) ;
#20019 = EDGE_CURVE ( 'NONE', #4165, #13876, #12947, .T. ) ;
#20018 = CYLINDRICAL_SURFACE ( 'NONE', #14173, 0.5000000000000000000 ) ;
#20020 = EDGE_CURVE ( 'NONE', #21815, #9771, #14237, .T. ) ;
#20021 = DIRECTION ( 'NONE',  ( 1.000000000000000000, 0.000000000000000000, 4.336808689941968432E-16 ) ) ;
#20022 = CARTESIAN_POINT ( 'NONE',  ( 4.163336342344337027E-14, 3.469446951953614189E-14, -3.000000000000002665 ) ) ;
#20023 = AXIS2_PLACEMENT_3D ( 'NONE', #15406, #22593, #8480 ) ;
#20024 = DIRECTION ( 'NONE',  ( 0.000000000000000000, 0.000000000000000000, 1.000000000000000000 ) ) ;
#20025 = CIRCLE ( 'NONE', #10998, 4.750000000000000000 ) ;
#20026 = DIRECTION ( 'NONE',  ( 4.844685039213900252E-16, 1.201780285297635172E-31, -1.000000000000000000 ) ) ;
#20027 = CIRCLE ( 'NONE', #18905, 0.2500000000000002220 ) ;
#20028 = CIRCLE ( 'NONE', #11382, 2.100000000000011635 ) ;
#20029 = CARTESIAN_POINT ( 'NONE',  ( 0.3263565795980739592, -4.430380094434307026, -5.351519936624962170 ) ) ;
#20030 = DIRECTION ( 'NONE',  ( -1.000000000000000000, -5.598259082250514647E-17, -3.330669073875432643E-16 ) ) ;
#20031 = CARTESIAN_POINT ( 'NONE',  ( 0.2174200650117543709, 2.185595227304866217, -3.214438021527934453 ) ) ;
#20032 = EDGE_CURVE ( 'NONE', #17450, #9641, #10817, .T. ) ;
#20033 = CARTESIAN_POINT ( 'NONE',  ( -4.330127018922199866, 4.999999999999920952, 7.500000000000007105 ) ) ;
#20034 = VERTEX_POINT ( 'NONE', #14120 ) ;
#20035 = EDGE_CURVE ( 'NONE', #17272, #7855, #4691, .T. ) ;
#20036 =( NAMED_UNIT ( * ) SI_UNIT ( $, .STERADIAN. ) SOLID_ANGLE_UNIT ( ) );
#20038 = EDGE_LOOP ( 'NONE', ( #18495, #22206, #19491, #13531 ) ) ;
#20037 = ORIENTED_EDGE ( 'NONE', *, *, #21380, .T. ) ;
#20039 = ADVANCED_FACE ( 'NONE', ( #12461 ), #21308, .T. ) ;
#20040 = ORIENTED_EDGE ( 'NONE', *, *, #15414, .F. ) ;
#20041 = ORIENTED_EDGE ( 'NONE', *, *, #12022, .T. ) ;
#20042 = AXIS2_PLACEMENT_3D ( 'NONE', #20829, #945, #21047 ) ;
#20044 = ORIENTED_EDGE ( 'NONE', *, *, #16010, .F. ) ;
#20043 = VERTEX_POINT ( 'NONE', #17766 ) ;
#20045 = VERTEX_POINT ( 'NONE', #1654 ) ;
#20046 = DIRECTION ( 'NONE',  ( 4.190823558986625216E-31, -1.000000000000000000, 4.190823558986625216E-31 ) ) ;
#20047 = CIRCLE ( 'NONE', #4237, 2.500000000000006661 ) ;
#20048 = ORIENTED_EDGE ( 'NONE', *, *, #18652, .F. ) ;
#20049 = TOROIDAL_SURFACE ( 'NONE', #14031, 5.500000000000000000, 0.5000000000000000000 ) ;
#20050 = ORIENTED_EDGE ( 'NONE', *, *, #22639, .T. ) ;
#20051 = AXIS2_PLACEMENT_3D ( 'NONE', #5206, #4733, #23214 ) ;
#20052 = CYLINDRICAL_SURFACE ( 'NONE', #5444, 0.5000000000000004441 ) ;
#20053 = CARTESIAN_POINT ( 'NONE',  ( 0.2499999999999655276, 2.000000000000015543, -1.500000000000001332 ) ) ;
#20054 = DIRECTION ( 'NONE',  ( -1.298062744027682297E-32, 6.902532920683810383E-31, -1.000000000000000000 ) ) ;
#20055 = DIRECTION ( 'NONE',  ( -2.220446049250313081E-16, 1.000000000000000000, -7.025792437124636392E-31 ) ) ;
#20056 = EDGE_CURVE ( 'NONE', #17226, #7345, #18216, .T. ) ;
#20057 = CYLINDRICAL_SURFACE ( 'NONE', #3488, 0.5000000000000017764 ) ;
#20058 = CARTESIAN_POINT ( 'NONE',  ( -2.500000000000002220, 1.793290614977871628E-14, -4.999999999999997335 ) ) ;
#20059 = CARTESIAN_POINT ( 'NONE',  ( -4.211140560182312420, 2.431303136016568889, -3.745885042887433958 ) ) ;
#20060 = DIRECTION ( 'NONE',  ( 0.9706398123736300620, 1.281898970984135951E-30, 0.2405376366294562085 ) ) ;
#20061 = DIRECTION ( 'NONE',  ( 0.000000000000000000, 0.000000000000000000, 1.000000000000000000 ) ) ;
#20062 = AXIS2_PLACEMENT_3D ( 'NONE', #21379, #3378, #19479 ) ;
#20063 = AXIS2_PLACEMENT_3D ( 'NONE', #10950, #21573, #19557 ) ;
#20064 = ADVANCED_FACE ( 'NONE', ( #21432 ), #19648, .F. ) ;
#20065 = CYLINDRICAL_SURFACE ( 'NONE', #18286, 3.000000000000000000 ) ;
#20066 = VECTOR ( 'NONE', #5142, 1000.000000000000000 ) ;
#20067 = ORIENTED_EDGE ( 'NONE', *, *, #17633, .F. ) ;
#20068 = FACE_OUTER_BOUND ( 'NONE', #21248, .T. ) ;
#20070 = EDGE_LOOP ( 'NONE', ( #6529, #19369 ) ) ;
#20069 = ORIENTED_EDGE ( 'NONE', *, *, #13413, .T. ) ;
#20071 = ADVANCED_FACE ( 'NONE', ( #1761, #14347 ), #16213, .T. ) ;
#20072 = ORIENTED_EDGE ( 'NONE', *, *, #14558, .T. ) ;
#20073 = ORIENTED_EDGE ( 'NONE', *, *, #22322, .F. ) ;
#20074 = EDGE_CURVE ( 'NONE', #3004, #1433, #18591, .T. ) ;
#20075 = EDGE_LOOP ( 'NONE', ( #19926, #21493, #15002, #8057 ) ) ;
#20076 = ORIENTED_EDGE ( 'NONE', *, *, #14489, .T. ) ;
#20077 = CARTESIAN_POINT ( 'NONE',  ( 88.75737332930593482, -6.527605602963476805, -6.499999999999929834 ) ) ;
#20078 = COLOUR_RGB ( '', 0.72549020, 0.75294118, 0.79215686) ;
#20079 = CLOSED_SHELL ( 'NONE', ( #2323, #1334, #8534, #17776, #10416, #11946, #3698, #15033, #8210, #16307, #207, #2571, #2494, #19444, #19891, #5279, #21863, #9513, #21608, #21880, #15563, #723, #14964, #18175, #17642, #2064, #8079, #15811, #11637, #3784, #15726, #20384, #4775, #15025, #10127, #9704, #5516, #22355, #13439, #3956, #12554, #898, #14133, #21742, #19791, #22053, #14941, #22533, #8592, #38, #20480, #11313, #9086, #20185, #20599, #6395, #22239, #3091, #5500, #1050, #10661, #16124, #21397, #1585, #2769, #21994, #4934, #16862, #15552, #6632, #6420, #18410, #2605, #13090, #16731, #1753, #19663, #1177, #14435, #11963, #6646, #3089, #9417, #10835, #1563, #19407 ) ) ;
#20080 = AXIS2_PLACEMENT_3D ( 'NONE', #18607, #14841, #9435 ) ;
#20081 = DIRECTION ( 'NONE',  ( 1.000000000000000000, -1.389842848855773367E-62, 2.013525853228507892E-32 ) ) ;
#20082 = AXIS2_PLACEMENT_3D ( 'NONE', #22416, #14999, #13363 ) ;
#20083 = CARTESIAN_POINT ( 'NONE',  ( 4.124214193018072905, -2.028338413290942555, -3.513185186763553514 ) ) ;
#20084 = CARTESIAN_POINT ( 'NONE',  ( -61.45000000000039364, -3.200000000000081890, -2.000000000000002220 ) ) ;
#20085 = DIRECTION ( 'NONE',  ( -1.000000000000000000, -6.224605580259554159E-31, 2.887593071917436153E-31 ) ) ;
#20086 = CARTESIAN_POINT ( 'NONE',  ( 7.518994333257404961, -11.74196038388119767, 8.837702940568448184 ) ) ;
#20087 = DIRECTION ( 'NONE',  ( -1.000000000000000000, 4.615739097524200579E-16, 1.134196829589820086E-15 ) ) ;
#20088 = CARTESIAN_POINT ( 'NONE',  ( -7.499999999999978684, -5.999999999999981348, 10.74999999999998224 ) ) ;
#20089 = DIRECTION ( 'NONE',  ( -1.000000000000000000, -4.440892098500626162E-16, 5.551115123125782702E-16 ) ) ;
#20090 = PLANE ( 'NONE',  #8029 ) ;
#20091 = EDGE_CURVE ( 'NONE', #2848, #6243, #17845, .T. ) ;
#20092 = FACE_BOUND ( 'NONE', #5244, .T. ) ;
#20093 = AXIS2_PLACEMENT_3D ( 'NONE', #5183, #5536, #17523 ) ;
#20094 = DIRECTION ( 'NONE',  ( 0.000000000000000000, -1.000000000000000000, 0.000000000000000000 ) ) ;
#20095 = CIRCLE ( 'NONE', #5076, 0.2500000000000000000 ) ;
#20096 = CARTESIAN_POINT ( 'NONE',  ( 3.958476099524783187, -1.406653531810735158, -3.500000000000010214 ) ) ;
#20097 = ADVANCED_FACE ( 'NONE', ( #12221 ), #1323, .T. ) ;
#20098 = ORIENTED_EDGE ( 'NONE', *, *, #21858, .F. ) ;
#20099 = CARTESIAN_POINT ( 'NONE',  ( -4.470458892752996682, 37.36863211987453326, -28.96516477595391592 ) ) ;
#20100 = ORIENTED_EDGE ( 'NONE', *, *, #1110, .T. ) ;
#20101 = CARTESIAN_POINT ( 'NONE',  ( 0.000000000000000000, 1.387778780781445676E-14, -10.86602540378443749 ) ) ;
#20102 = CARTESIAN_POINT ( 'NONE',  ( -6.938893903907228378E-14, -4.618802153517020059, -5.242734410091827613 ) ) ;
#20103 = CARTESIAN_POINT ( 'NONE',  ( 3.958484000407251457, -3.734437307742051182, -0.5317648453101290196 ) ) ;
#20104 = DIRECTION ( 'NONE',  ( 1.000000000000000000, 1.910522504832140594E-31, -5.551115123125818447E-17 ) ) ;
#20105 = CARTESIAN_POINT ( 'NONE',  ( 6.844222713676473743E-15, 4.618802153517023612, -3.504269196027541167 ) ) ;
#20106 = AXIS2_PLACEMENT_3D ( 'NONE', #17757, #1646, #8473 ) ;
#20107 = DIRECTION ( 'NONE',  ( -0.000000000000000000, -0.000000000000000000, 1.000000000000000000 ) ) ;
#20108 = DIRECTION ( 'NONE',  ( -2.220446049250313081E-16, 1.000000000000000000, -7.025792437124636392E-31 ) ) ;
#20109 = CARTESIAN_POINT ( 'NONE',  ( 3.366108932388589547E-15, 0.3423821193476806468, -3.500000000000009326 ) ) ;
#20110 = CARTESIAN_POINT ( 'NONE',  ( 77.42435809754134368, -10.99999999999981526, -6.000000000000047073 ) ) ;
#20111 = CARTESIAN_POINT ( 'NONE',  ( -90.55603112840530855, 2.700000000000056577, -7.432974388601742533 ) ) ;
#20112 = CARTESIAN_POINT ( 'NONE',  ( 0.1388410611046139165, -3.710337782248038341, -0.5735064479039801988 ) ) ;
#20113 = EDGE_LOOP ( 'NONE', ( #12710, #20073, #16942, #7509 ) ) ;
#20114 = CARTESIAN_POINT ( 'NONE',  ( 2.775557561562891351E-14, 10.99999999999998579, -0.4999999999999865663 ) ) ;
#20115 = CARTESIAN_POINT ( 'NONE',  ( 2.500000000000000000, 2.570099380655443508E-14, 1.965053746192312752E-17 ) ) ;
#20116 = DIRECTION ( 'NONE',  ( 1.000000000000000000, 2.699383410053119644E-30, 3.330669073875432643E-16 ) ) ;
#20117 = DIRECTION ( 'NONE',  ( 1.000000000000000000, 4.440892098500626162E-16, -5.551115123125782702E-16 ) ) ;
#20118 = B_SPLINE_CURVE_WITH_KNOTS ( 'NONE', 3,
 ( #17267, #15270, #13640, #10333, #6809, #9878, #18937, #20937 ),
 .UNSPECIFIED., .F., .F.,
 ( 4, 2, 2, 4 ),
 ( 2.465131516885230102E-07, 0.001183067374689851514, 0.001774477805458931972, 0.002365888236228012864 ),
 .UNSPECIFIED. ) ;
#20119 = SHAPE_DEFINITION_REPRESENTATION ( #3109, #22944 ) ;
#20120 = TOROIDAL_SURFACE ( 'NONE', #3960, 6.000000000000000000, 0.5000000000000000000 ) ;
#20121 = EDGE_LOOP ( 'NONE', ( #17504, #3385, #744, #9456, #3209, #20661, #14228, #12743 ) ) ;
#20122 = PRODUCT_DEFINITION ( 'UNKNOWN', '', #10, #2752 ) ;
#20124 = ORIENTED_EDGE ( 'NONE', *, *, #8436, .T. ) ;
#20123 = EDGE_LOOP ( 'NONE', ( #7907, #2672 ) ) ;
#20125 = CARTESIAN_POINT ( 'NONE',  ( 12.84999999999997300, -12.00000000000005151, 2.550000000000038902 ) ) ;
#20126 = DIRECTION ( 'NONE',  ( -1.000000000000000000, 1.445602896647327823E-16, 0.000000000000000000 ) ) ;
#20127 = EDGE_CURVE ( 'NONE', #16517, #6243, #13342, .T. ) ;
#20128 = CARTESIAN_POINT ( 'NONE',  ( 6.999999991928306464, -11.17450167042447617, 8.700799235122161690 ) ) ;
#20129 = ORIENTED_EDGE ( 'NONE', *, *, #6144, .T. ) ;
#20130 = AXIS2_PLACEMENT_3D ( 'NONE', #9894, #964, #15292 ) ;
#20131 = CARTESIAN_POINT ( 'NONE',  ( -4.690415759824456465, -0.7499999999999242828, -1.999999999999849010 ) ) ;
#20132 = DIRECTION ( 'NONE',  ( -1.000000000000000000, -3.254448077276381206E-32, -1.066788928082016908E-26 ) ) ;
#20133 = DIRECTION ( 'NONE',  ( -1.000000000000000000, 0.000000000000000000, -4.336808689941968432E-16 ) ) ;
#20134 = CARTESIAN_POINT ( 'NONE',  ( 1.200000000000006617, -0.5999999999999963141, -4.543283425070376857 ) ) ;
#20135 = DIRECTION ( 'NONE',  ( -0.7313537016191730133, 0.6819983600624958120, -5.924440990721418971E-17 ) ) ;
#20136 = EDGE_CURVE ( 'NONE', #1206, #195, #16317, .T. ) ;
#20137 = DIRECTION ( 'NONE',  ( -7.860214984770699307E-18, 1.409037165336591006E-16, 1.000000000000000000 ) ) ;
#20138 = DIRECTION ( 'NONE',  ( 1.066786462891689527E-26, 6.656013887802287108E-31, 1.000000000000000000 ) ) ;
#20139 = CYLINDRICAL_SURFACE ( 'NONE', #3909, 2.000000000000000000 ) ;
#20140 = CARTESIAN_POINT ( 'NONE',  ( 2.918498775983380256E-10, 2.999999999003851503, -15.99999999999999289 ) ) ;
#20141 = CARTESIAN_POINT ( 'NONE',  ( 2.500000000000015543, -2.885729496010487183E-15, -4.974599999999995248 ) ) ;
#20142 = DIRECTION ( 'NONE',  ( -1.000000000000000000, -1.479114197289387852E-30, 2.013525853228518840E-32 ) ) ;
#20143 = CIRCLE ( 'NONE', #20538, 2.000000000000015543 ) ;
#20144 = B_SPLINE_CURVE_WITH_KNOTS ( 'NONE', 3,
 ( #10533, #15813, #80, #21132, #5124 ),
 .UNSPECIFIED., .F., .F.,
 ( 4, 1, 4 ),
 ( 0.000000000000000000, 0.002020725942163687904, 0.004041451884327375808 ),
 .UNSPECIFIED. ) ;
#20145 = CARTESIAN_POINT ( 'NONE',  ( 0.000000000000000000, 0.000000000000000000, -5.294516984716112873 ) ) ;
#20146 = DIRECTION ( 'NONE',  ( -0.7071067811865475727, 0.7071067811865475727, 0.000000000000000000 ) ) ;
#20147 = FACE_OUTER_BOUND ( 'NONE', #8143, .T. ) ;
#20148 = VERTEX_POINT ( 'NONE', #2455 ) ;
#20149 = AXIS2_PLACEMENT_3D ( 'NONE', #17501, #9037, #14451 ) ;
#20150 = SHAPE_REPRESENTATION_RELATIONSHIP ( 'NONE' , 'NONE' ,  #14072, #202 ) ;
#20152 = ORIENTED_EDGE ( 'NONE', *, *, #4941, .F. ) ;
#20151 = ORIENTED_EDGE ( 'NONE', *, *, #1184, .T. ) ;
#20153 = UNCERTAINTY_MEASURE_WITH_UNIT (LENGTH_MEASURE( 1.000000000000000082E-05 ), #1627, 'distance_accuracy_value', 'NONE');
#20154 = ORIENTED_EDGE ( 'NONE', *, *, #10947, .F. ) ;
#20155 = EDGE_CURVE ( 'NONE', #4546, #20884, #7639, .T. ) ;
#20156 = VERTEX_POINT ( 'NONE', #7753 ) ;
#20158 = ORIENTED_EDGE ( 'NONE', *, *, #17610, .F. ) ;
#20157 = ORIENTED_EDGE ( 'NONE', *, *, #21508, .T. ) ;
#20159 = ORIENTED_EDGE ( 'NONE', *, *, #17270, .T. ) ;
#20160 = FACE_OUTER_BOUND ( 'NONE', #22359, .T. ) ;
#20161 = VERTEX_POINT ( 'NONE', #18113 ) ;
#20162 = EDGE_CURVE ( 'NONE', #13948, #12565, #9189, .T. ) ;
#20163 = EDGE_LOOP ( 'NONE', ( #1160, #11026, #19023, #16436 ) ) ;
#20164 = DIRECTION ( 'NONE',  ( 1.815210279346896549E-30, -6.902532920684321857E-31, 1.000000000000000000 ) ) ;
#20165 = VECTOR ( 'NONE', #10889, 1000.000000000000000 ) ;
#20166 = CARTESIAN_POINT ( 'NONE',  ( -0.6666666666667374619, -4.233901974057366679, -3.300726591567110013 ) ) ;
#20167 = CARTESIAN_POINT ( 'NONE',  ( 37.43301270189239460, 10.75000000000000000, -6.500000000000019540 ) ) ;
#20168 = CARTESIAN_POINT ( 'NONE',  ( -7.568091547083694692, -2.695633093451115680, 8.516664522246127689 ) ) ;
#20169 = CONICAL_SURFACE ( 'NONE', #4757, 4.750000000000000000, 1.047197551196600074 ) ;
#20170 = EDGE_CURVE ( 'NONE', #6591, #18554, #2046, .T. ) ;
#20171 = CARTESIAN_POINT ( 'NONE',  ( 0.3126073911696447549, 2.020725942163625888, -3.499999999999996003 ) ) ;
#20172 = CARTESIAN_POINT ( 'NONE',  ( 1.110223024625156540E-13, 1.749999999999998002, -4.750000000000000888 ) ) ;
#20173 = EDGE_CURVE ( 'NONE', #16292, #4603, #13171, .T. ) ;
#20174 = CARTESIAN_POINT ( 'NONE',  ( 29.00000000029184832, 16.99999999900385461, -29.00000000000000355 ) ) ;
#20175 = CARTESIAN_POINT ( 'NONE',  ( 2.000000000000029310, 3.464101615137740175, -5.600000000000000533 ) ) ;
#20176 = FACE_BOUND ( 'NONE', #23065, .T. ) ;
#20177 = CARTESIAN_POINT ( 'NONE',  ( 4.113620667976089607, -1.750000000000025757, 2.374999999999986677 ) ) ;
#20178 = VERTEX_POINT ( 'NONE', #12811 ) ;
#20179 = PRODUCT_DEFINITION_CONTEXT ( 'detailed design', #19150, 'design' ) ;
#20180 = VECTOR ( 'NONE', #14863, 1000.000000000000000 ) ;
#20181 =( NAMED_UNIT ( * ) SI_UNIT ( $, .STERADIAN. ) SOLID_ANGLE_UNIT ( ) );
#20182 = FACE_OUTER_BOUND ( 'NONE', #12796, .T. ) ;
#20184 = ORIENTED_EDGE ( 'NONE', *, *, #1058, .F. ) ;
#20183 = ORIENTED_EDGE ( 'NONE', *, *, #1071, .T. ) ;
#20185 = ADVANCED_FACE ( 'NONE', ( #14582 ), #404, .T. ) ;
#20186 = VECTOR ( 'NONE', #4357, 1000.000000000000000 ) ;
#20187 = ORIENTED_EDGE ( 'NONE', *, *, #13742, .T. ) ;
#20188 = ADVANCED_FACE ( 'NONE', ( #8103 ), #20579, .T. ) ;
#20189 = EDGE_CURVE ( 'NONE', #7230, #882, #6456, .T. ) ;
#20190 = VECTOR ( 'NONE', #22723, 1000.000000000000000 ) ;
#20191 = ORIENTED_EDGE ( 'NONE', *, *, #22325, .F. ) ;
#20192 = AXIS2_PLACEMENT_3D ( 'NONE', #22129, #7551, #3896 ) ;
#20193 = ORIENTED_EDGE ( 'NONE', *, *, #8520, .T. ) ;
#20194 = ORIENTED_EDGE ( 'NONE', *, *, #4180, .T. ) ;
#20195 = LINE ( 'NONE', #5730, #19299 ) ;
#20196 = CIRCLE ( 'NONE', #7053, 2.000000000000015543 ) ;
#20197 = B_SPLINE_CURVE_WITH_KNOTS ( 'NONE', 3,
 ( #14236, #14117, #16210, #3645, #18004, #10812, #10915, #8707, #9174, #1867 ),
 .UNSPECIFIED., .F., .F.,
 ( 4, 2, 2, 2, 4 ),
 ( 0.008003515366661734937, 0.008517983447693508806, 0.009032451528725282675, 0.009546919609757058278, 0.01006138769078883388 ),
 .UNSPECIFIED. ) ;
#20198 = DIRECTION ( 'NONE',  ( 1.000000000000000000, -4.190823558986610327E-31, 1.733449886265890494E-32 ) ) ;
#20199 = EDGE_CURVE ( 'NONE', #18669, #19569, #15262, .T. ) ;
#20200 = CARTESIAN_POINT ( 'NONE',  ( 37.86602540378461157, 0.000000000000000000, -10.86602540378449255 ) ) ;
#20201 = EDGE_CURVE ( 'NONE', #11516, #14827, #2925, .T. ) ;
#20202 = DIRECTION ( 'NONE',  ( 1.000000000000000000, -5.551115122690158919E-17, 1.001543064812511222E-16 ) ) ;
#20203 = DIRECTION ( 'NONE',  ( -2.168404344971017743E-16, 1.000000000000000000, 7.722382221513089478E-47 ) ) ;
#20204 = CIRCLE ( 'NONE', #4789, 4.499999999999988454 ) ;
#20205 = DIRECTION ( 'NONE',  ( 0.2405376366294550983, 0.000000000000000000, -0.9706398123736303951 ) ) ;
#20206 = CARTESIAN_POINT ( 'NONE',  ( -7.901093513163778503, -12.32682690073933252, 7.745538272134556479 ) ) ;
#20207 = CIRCLE ( 'NONE', #10054, 4.000000000000045297 ) ;
#20208 = CARTESIAN_POINT ( 'NONE',  ( -7.499999999999992006, -12.60977222864646485, 9.250000000000071054 ) ) ;
#20209 = CARTESIAN_POINT ( 'NONE',  ( 0.000000000000000000, 0.000000000000000000, -5.000000000000000888 ) ) ;
#20210 = CARTESIAN_POINT ( 'NONE',  ( -12.85000000000002807, -12.50000000000002842, 6.250000000000061284 ) ) ;
#20211 = AXIS2_PLACEMENT_3D ( 'NONE', #18572, #5764, #14806 ) ;
#20212 = DIRECTION ( 'NONE',  ( 2.172745813409349776E-17, -1.000000000000000000, 1.309377075419428048E-16 ) ) ;
#20213 = SHAPE_REPRESENTATION_RELATIONSHIP ( 'NONE' , 'NONE' ,  #20536, #15045 ) ;
#20214 = DIRECTION ( 'NONE',  ( 0.000000000000000000, 0.000000000000000000, 1.000000000000000000 ) ) ;
#20215 = DIRECTION ( 'NONE',  ( -0.4999999999999999445, -4.767331059895059913E-16, -0.8660254037844387076 ) ) ;
#20216 = ORIENTED_EDGE ( 'NONE', *, *, #19558, .F. ) ;
#20217 = CIRCLE ( 'NONE', #1420, 5.500000000000000000 ) ;
#20218 = VECTOR ( 'NONE', #8167, 1000.000000000000114 ) ;
#20219 = CARTESIAN_POINT ( 'NONE',  ( -4.149603749300068145, 38.03274690132711555, -28.99686245475831470 ) ) ;
#20220 = FACE_OUTER_BOUND ( 'NONE', #2643, .T. ) ;
#20221 = ORIENTED_EDGE ( 'NONE', *, *, #3592, .F. ) ;
#20222 = VERTEX_POINT ( 'NONE', #11623 ) ;
#20224 = VECTOR ( 'NONE', #10892, 1000.000000000000000 ) ;
#20223 =( REPRESENTATION_RELATIONSHIP ('NONE','NONE', #19450, #22944 ) REPRESENTATION_RELATIONSHIP_WITH_TRANSFORMATION ( #22581 )SHAPE_REPRESENTATION_RELATIONSHIP( ) );
#20225 = LINE ( 'NONE', #18445, #6532 ) ;
#20226 = EDGE_CURVE ( 'NONE', #10173, #14506, #9208, .T. ) ;
#20227 = FACE_OUTER_BOUND ( 'NONE', #13673, .T. ) ;
#20228 = CARTESIAN_POINT ( 'NONE',  ( 2.130086964121800697E-14, 3.273442688548750448E-16, 2.500000000000000000 ) ) ;
#20229 = DIRECTION ( 'NONE',  ( -1.000000000000000000, -2.220446049250318011E-16, 0.000000000000000000 ) ) ;
#20230 =( GEOMETRIC_REPRESENTATION_CONTEXT ( 3 ) GLOBAL_UNCERTAINTY_ASSIGNED_CONTEXT ( ( #7455 ) ) GLOBAL_UNIT_ASSIGNED_CONTEXT ( ( #17648, #3316, #14008 ) ) REPRESENTATION_CONTEXT ( 'NONE', 'WORKASPACE' ) );
#20231 = DIRECTION ( 'NONE',  ( 0.7313537016191730133, -0.6819983600624959230, 5.924440990721418971E-17 ) ) ;
#20232 = TOROIDAL_SURFACE ( 'NONE', #19855, 2.250000000000000444, 0.2500000000000000000 ) ;
#20233 = CARTESIAN_POINT ( 'NONE',  ( -12.85000000000001386, -12.00000000000006928, 4.163336342344337027E-14 ) ) ;
#20234 = CARTESIAN_POINT ( 'NONE',  ( 0.000000000000000000, -4.618802153517061804, -5.600000000000000533 ) ) ;
#20235 = EDGE_CURVE ( 'NONE', #16467, #13441, #17262, .T. ) ;
#20236 = CARTESIAN_POINT ( 'NONE',  ( 7.000000000000020428, -13.21292803502076652, 9.239863038076370216 ) ) ;
#20237 = CARTESIAN_POINT ( 'NONE',  ( 7.748687480237922642, -13.73110298228169590, 8.040801957829224023 ) ) ;
#20238 = DIRECTION ( 'NONE',  ( -1.066811114794977684E-26, 0.000000000000000000, -1.000000000000000000 ) ) ;
#20239 = LINE ( 'NONE', #7755, #6566 ) ;
#20240 = CARTESIAN_POINT ( 'NONE',  ( 7.596194078004423034, 47.59619407671642222, -18.50000000000000355 ) ) ;
#20241 = SURFACE_STYLE_USAGE ( .BOTH. , #4212 ) ;
#20242 = VECTOR ( 'NONE', #20374, 1000.000000000000000 ) ;
#20243 = CARTESIAN_POINT ( 'NONE',  ( 4.055492966679413058, -2.385006769472238108, -3.005124364834172113 ) ) ;
#20244 = TOROIDAL_SURFACE ( 'NONE', #2956, 4.500000000000000888, 0.5000000000000000000 ) ;
#20245 = PRODUCT_CONTEXT ( 'NONE', #19880, 'mechanical' ) ;
#20246 = CIRCLE ( 'NONE', #22494, 5.500000000000032863 ) ;
#20247 = ORIENTED_EDGE ( 'NONE', *, *, #22469, .F. ) ;
#20249 = EDGE_LOOP ( 'NONE', ( #21611, #8720, #1124, #5228 ) ) ;
#20248 = ORIENTED_EDGE ( 'NONE', *, *, #19324, .F. ) ;
#20250 = CARTESIAN_POINT ( 'NONE',  ( -95.70000000000069917, 2.775557561562891351E-14, 8.000000000000090594 ) ) ;
#20251 = MECHANICAL_DESIGN_GEOMETRIC_PRESENTATION_REPRESENTATION (  '', ( #22873 ), #18007 ) ;
#20252 = CARTESIAN_POINT ( 'NONE',  ( 7.835312244869989229, -0.05103360697234643473, 7.041165740960562580 ) ) ;
#20253 = FACE_OUTER_BOUND ( 'NONE', #15312, .T. ) ;
#20254 = ORIENTED_EDGE ( 'NONE', *, *, #11233, .T. ) ;
#20255 = CARTESIAN_POINT ( 'NONE',  ( 4.114405500665264448, 4.051151509359390168, 6.940203675128279408E-15 ) ) ;
#20256 = LINE ( 'NONE', #4119, #6773 ) ;
#20257 = DIRECTION ( 'NONE',  ( 0.7071067811865490160, 0.7071067811865460184, 1.565905175853767167E-16 ) ) ;
#20258 = DIRECTION ( 'NONE',  ( 2.013525853228507892E-32, 6.902532920683810383E-31, -1.000000000000000000 ) ) ;
#20259 = AXIS2_PLACEMENT_3D ( 'NONE', #16168, #22906, #3381 ) ;
#20260 = CARTESIAN_POINT ( 'NONE',  ( 33.94974746859769255, 21.94974746730969528, -25.50000000000000355 ) ) ;
#20261 = TOROIDAL_SURFACE ( 'NONE', #10114, 5.750000000000000000, 0.5000000000000000000 ) ;
#20262 = CARTESIAN_POINT ( 'NONE',  ( 4.000000000000003553, 0.000000000000000000, -5.600000000000000533 ) ) ;
#20263 = CARTESIAN_POINT ( 'NONE',  ( 2.918498775983380256E-10, 5.999999999003851059, -32.00000000000000000 ) ) ;
#20264 = SURFACE_STYLE_FILL_AREA ( #13079 ) ;
#20265 = FACE_OUTER_BOUND ( 'NONE', #18161, .T. ) ;
#20266 = LINE ( 'NONE', #4128, #12652 ) ;
#20267 = CARTESIAN_POINT ( 'NONE',  ( -6.999999999999992006, -8.000000000000044409, 6.250000000000019540 ) ) ;
#20268 = DIRECTION ( 'NONE',  ( 5.551115123125782702E-16, 1.201780285297635172E-31, -1.000000000000000000 ) ) ;
#20269 = CARTESIAN_POINT ( 'NONE',  ( -55.05572809000125289, -0.5000000000001045830, -10.00000000000006395 ) ) ;
#20270 =( GEOMETRIC_REPRESENTATION_CONTEXT ( 3 ) GLOBAL_UNCERTAINTY_ASSIGNED_CONTEXT ( ( #7935 ) ) GLOBAL_UNIT_ASSIGNED_CONTEXT ( ( #9094, #6033, #5690 ) ) REPRESENTATION_CONTEXT ( 'NONE', 'WORKASPACE' ) );
#20271 = VERTEX_POINT ( 'NONE', #16909 ) ;
#20272 = ADVANCED_FACE ( 'NONE', ( #9757 ), #12196, .F. ) ;
#20273 = SURFACE_STYLE_USAGE ( .BOTH. , #5914 ) ;
#20275 = ORIENTED_EDGE ( 'NONE', *, *, #9390, .F. ) ;
#20274 = ORIENTED_EDGE ( 'NONE', *, *, #19117, .T. ) ;
#20276 = ORIENTED_EDGE ( 'NONE', *, *, #17482, .F. ) ;
#20277 = ORIENTED_EDGE ( 'NONE', *, *, #18366, .F. ) ;
#20279 = VERTEX_POINT ( 'NONE', #11740 ) ;
#20278 = ORIENTED_EDGE ( 'NONE', *, *, #12130, .F. ) ;
#20280 = EDGE_LOOP ( 'NONE', ( #19449, #7571, #63, #16200 ) ) ;
#20281 = CARTESIAN_POINT ( 'NONE',  ( 12.84999999999997300, -1.999999999999998224, 0.000000000000000000 ) ) ;
#20282 = ORIENTED_EDGE ( 'NONE', *, *, #22962, .F. ) ;
#20283 = ORIENTED_EDGE ( 'NONE', *, *, #7385, .T. ) ;
#20284 = CARTESIAN_POINT ( 'NONE',  ( 119.5756419024615838, -6.500000000000005329, 6.000000000000158096 ) ) ;
#20285 = AXIS2_PLACEMENT_3D ( 'NONE', #5174, #14114, #10344 ) ;
#20286 = DIRECTION ( 'NONE',  ( -1.393974221767077062E-14, -1.000000000000000000, 0.000000000000000000 ) ) ;
#20287 = DIRECTION ( 'NONE',  ( 1.000000000000000000, 0.000000000000000000, 0.000000000000000000 ) ) ;
#20288 = DIRECTION ( 'NONE',  ( -2.220446049250313081E-16, 1.000000000000000000, -7.025792437124636392E-31 ) ) ;
#20289 = CARTESIAN_POINT ( 'NONE',  ( -12.85000000000002807, -13.50000000000003020, 6.250000000000033751 ) ) ;
#20290 = CYLINDRICAL_SURFACE ( 'NONE', #22276, 2.500000000000001332 ) ;
#20291 = DIRECTION ( 'NONE',  ( 2.775557561562885188E-17, 1.309377075419427801E-16, 1.000000000000000000 ) ) ;
#20292 = CARTESIAN_POINT ( 'NONE',  ( -2.428612866367529932E-14, 2.000000000000043521, -19.00000000000001066 ) ) ;
#20293 = FILL_AREA_STYLE ('',( #14873 ) ) ;
#20294 = CARTESIAN_POINT ( 'NONE',  ( 2.036182501904611954E-14, 0.3423821193476729863, -3.500000000000035527 ) ) ;
#20295 = LINE ( 'NONE', #4159, #8142 ) ;
#20296 = ORIENTED_EDGE ( 'NONE', *, *, #3523, .F. ) ;
#20297 = ADVANCED_FACE ( 'NONE', ( #2684 ), #23126, .T. ) ;
#20298 = CARTESIAN_POINT ( 'NONE',  ( 33.94974746859769255, 21.94974746730969528, -18.50000000000000355 ) ) ;
#20299 = VECTOR ( 'NONE', #8041, 1000.000000000000000 ) ;
#20301 = ORIENTED_EDGE ( 'NONE', *, *, #1339, .F. ) ;
#20300 = ORIENTED_EDGE ( 'NONE', *, *, #16858, .T. ) ;
#20302 = EDGE_LOOP ( 'NONE', ( #22032, #18794, #17425 ) ) ;
#20303 = EDGE_CURVE ( 'NONE', #16865, #19136, #22698, .T. ) ;
#20304 = ORIENTED_EDGE ( 'NONE', *, *, #1744, .F. ) ;
#20305 = EDGE_CURVE ( 'NONE', #749, #21173, #15596, .T. ) ;
#20306 = EDGE_CURVE ( 'NONE', #12739, #6667, #6971, .T. ) ;
#20307 = ORIENTED_EDGE ( 'NONE', *, *, #7782, .F. ) ;
#20308 = CARTESIAN_POINT ( 'NONE',  ( 0.000000000000000000, 4.041451884327383226, -1.734723475976807094E-15 ) ) ;
#20309 = FACE_OUTER_BOUND ( 'NONE', #7968, .T. ) ;
#20310 = EDGE_LOOP ( 'NONE', ( #17302, #21472, #23091, #16398 ) ) ;
#20311 = CARTESIAN_POINT ( 'NONE',  ( 4.175813232069149450, -4.122719923832729449, 0.000000000000000000 ) ) ;
#20312 = FACE_OUTER_BOUND ( 'NONE', #20421, .T. ) ;
#20313 = LINE ( 'NONE', #4177, #21778 ) ;
#20314 = VECTOR ( 'NONE', #2249, 1000.000000000000000 ) ;
#20315 = CARTESIAN_POINT ( 'NONE',  ( -8.660254037844428154, 4.689110867544629357, -1.387778780781445676E-14 ) ) ;
#20316 = CARTESIAN_POINT ( 'NONE',  ( -7.602880770961808032, -11.99349919129478792, 8.461619612152084358 ) ) ;
#20317 = EDGE_CURVE ( 'NONE', #11317, #10432, #8468, .T. ) ;
#20318 = CARTESIAN_POINT ( 'NONE',  ( -7.176407415342067608, -13.63581929081302313, 8.314790908397574398 ) ) ;
#20319 = DIRECTION ( 'NONE',  ( 0.000000000000000000, 0.000000000000000000, 1.000000000000000000 ) ) ;
#20320 = CARTESIAN_POINT ( 'NONE',  ( -6.000000000000074607, -4.800000000000026468, -7.500000000000034639 ) ) ;
#20321 = FACE_OUTER_BOUND ( 'NONE', #18017, .T. ) ;
#20322 = PRESENTATION_STYLE_ASSIGNMENT (( #2434 ) ) ;
#20323 = DIRECTION ( 'NONE',  ( 1.733449886265891589E-32, -4.190823558986610327E-31, 1.000000000000000000 ) ) ;
#20324 = CARTESIAN_POINT ( 'NONE',  ( 3.950233766685289361, 0.7256672287178125291, -3.499999999999854339 ) ) ;
#20325 = VERTEX_POINT ( 'NONE', #19153 ) ;
#20326 = ADVANCED_FACE ( 'NONE', ( #10204 ), #1287, .T. ) ;
#20327 = EDGE_CURVE ( 'NONE', #14506, #8601, #953, .T. ) ;
#20328 = ORIENTED_EDGE ( 'NONE', *, *, #2470, .T. ) ;
#20329 = ORIENTED_EDGE ( 'NONE', *, *, #5967, .F. ) ;
#20330 = EDGE_CURVE ( 'NONE', #4062, #8320, #20871, .T. ) ;
#20331 = DIRECTION ( 'NONE',  ( 0.9878135252003128475, -1.532010627492774680E-16, -0.1556420233463030045 ) ) ;
#20332 = CARTESIAN_POINT ( 'NONE',  ( -4.000000000000003553, -2.309401076758532678, -5.242734410091827613 ) ) ;
#20333 = ORIENTED_EDGE ( 'NONE', *, *, #12703, .F. ) ;
#20334 = DIRECTION ( 'NONE',  ( 0.000000000000000000, 0.000000000000000000, 1.000000000000000000 ) ) ;
#20335 = DIRECTION ( 'NONE',  ( -1.550910762415566494E-16, -1.000000000000000000, 8.135128085091684243E-31 ) ) ;
#20336 = PLANE ( 'NONE',  #1579 ) ;
#20337 = DIRECTION ( 'NONE',  ( -9.121204216617949000E-31, -1.000000000000000000, 6.982962677686261977E-15 ) ) ;
#20338 = CARTESIAN_POINT ( 'NONE',  ( -64.00000000000045475, 3.200000000000057021, -1.999999999999974021 ) ) ;
#20339 = CARTESIAN_POINT ( 'NONE',  ( -64.00000000000038369, -2.700000000000091216, -2.000000000000029310 ) ) ;
#20340 = CARTESIAN_POINT ( 'NONE',  ( -6.959810536856695151, 36.00015702695179698, -18.51059057611807646 ) ) ;
#20341 = CARTESIAN_POINT ( 'NONE',  ( 7.490952241692768077, -13.34551170378462537, 8.992386117842924520 ) ) ;
#20342 = DIRECTION ( 'NONE',  ( -9.693522803355793065E-26, 5.963788443470849249E-28, 1.000000000000000000 ) ) ;
#20343 = AXIS2_PLACEMENT_3D ( 'NONE', #7495, #5273, #21404 ) ;
#20344 = AXIS2_PLACEMENT_3D ( 'NONE', #20369, #15059, #4238 ) ;
#20345 = FACE_OUTER_BOUND ( 'NONE', #16150, .T. ) ;
#20346 = DIRECTION ( 'NONE',  ( -1.129541670263356189E-15, -6.741645191078037727E-32, 1.000000000000000000 ) ) ;
#20347 = FILL_AREA_STYLE_COLOUR ( '', #9619 ) ;
#20348 = DIRECTION ( 'NONE',  ( 1.000000000000000000, 3.254448077276381206E-32, 1.066788928082016908E-26 ) ) ;
#20349 = EDGE_CURVE ( 'NONE', #5046, #12160, #15155, .T. ) ;
#20350 = ITEM_DEFINED_TRANSFORMATION ( 'NONE', 'NONE', #9385,  #22115 ) ;
#20351 = ORIENTED_EDGE ( 'NONE', *, *, #6503, .T. ) ;
#20352 = EDGE_CURVE ( 'NONE', #22294, #14175, #580, .T. ) ;
#20354 = ORIENTED_EDGE ( 'NONE', *, *, #18187, .F. ) ;
#20353 = ORIENTED_EDGE ( 'NONE', *, *, #3219, .T. ) ;
#20355 = CIRCLE ( 'NONE', #1566, 0.4999999999999978351 ) ;
#20356 = DIRECTION ( 'NONE',  ( 1.000000000000000000, 1.725633230170952464E-30, -1.831867990631496853E-15 ) ) ;
#20357 = CARTESIAN_POINT ( 'NONE',  ( 24.99999999999998934, 1.500000000000001332, 0.000000000000000000 ) ) ;
#20358 = CARTESIAN_POINT ( 'NONE',  ( 6.938893903907228378E-15, 4.618802153517023612, -5.000000000000000888 ) ) ;
#20359 = ORIENTED_EDGE ( 'NONE', *, *, #3079, .T. ) ;
#20360 = CARTESIAN_POINT ( 'NONE',  ( 4.158413352280808439, 4.089743253945565371, 3.469446951953614189E-15 ) ) ;
#20361 = DIRECTION ( 'NONE',  ( -9.693457064947022734E-26, 0.000000000000000000, 1.000000000000000000 ) ) ;
#20362 = CARTESIAN_POINT ( 'NONE',  ( 4.093692494532772841, -2.021783646005771207, 3.501831996793841384 ) ) ;
#20363 = CARTESIAN_POINT ( 'NONE',  ( -42.54314575050793934, 3.999999999999996447, 7.500000000000062172 ) ) ;
#20364 = DIRECTION ( 'NONE',  ( 8.438582421954110511E-32, 0.000000000000000000, 1.000000000000000000 ) ) ;
#20365 = CIRCLE ( 'NONE', #1217, 3.500000000000004441 ) ;
#20366 = CARTESIAN_POINT ( 'NONE',  ( -4.163336342344337027E-14, 2.081668171172168513E-14, 10.24999999999993960 ) ) ;
#20367 = CARTESIAN_POINT ( 'NONE',  ( -0.7206956945560699657, 4.999999999999962697, 7.500000000000007994 ) ) ;
#20368 = FACE_OUTER_BOUND ( 'NONE', #10537, .T. ) ;
#20369 = CARTESIAN_POINT ( 'NONE',  ( -6.938893903907228378E-15, 1.500000000000001332, 0.000000000000000000 ) ) ;
#20370 = ADVANCED_FACE ( 'NONE', ( #6689 ), #3508, .T. ) ;
#20371 = DIRECTION ( 'NONE',  ( -2.013525853228507892E-32, -6.902532920683810383E-31, 1.000000000000000000 ) ) ;
#20372 = DIRECTION ( 'NONE',  ( -9.121204216617949000E-31, -1.000000000000000000, 6.982962677686261977E-15 ) ) ;
#20373 = AXIS2_PLACEMENT_3D ( 'NONE', #14891, #10175, #2774 ) ;
#20374 = DIRECTION ( 'NONE',  ( -0.7313537016191746787, -0.6819983600624940356, -1.072890437865584409E-16 ) ) ;
#20376 = CIRCLE ( 'NONE', #6490, 4.000000000000045297 ) ;
#20375 = DIRECTION ( 'NONE',  ( -0.000000000000000000, 1.000000000000000000, -0.000000000000000000 ) ) ;
#20377 = ADVANCED_FACE ( 'NONE', ( #7046 ), #3281, .F. ) ;
#20378 = CIRCLE ( 'NONE', #6470, 0.2500000000000002220 ) ;
#20379 = ORIENTED_EDGE ( 'NONE', *, *, #21934, .F. ) ;
#20380 = DIRECTION ( 'NONE',  ( 0.7296441571687835026, 0.6838270277705145173, -7.592084613012316059E-17 ) ) ;
#20382 = VERTEX_POINT ( 'NONE', #6928 ) ;
#20381 = EDGE_LOOP ( 'NONE', ( #6500, #3087, #14313, #624, #21062 ) ) ;
#20383 = UNCERTAINTY_MEASURE_WITH_UNIT (LENGTH_MEASURE( 1.000000000000000082E-05 ), #17649, 'distance_accuracy_value', 'NONE');
#20384 = ADVANCED_FACE ( 'NONE', ( #4905 ), #16187, .F. ) ;
#20385 = EDGE_LOOP ( 'NONE', ( #13356, #14132, #4950, #1270 ) ) ;
#20387 = EDGE_LOOP ( 'NONE', ( #13931, #16866, #19190, #18059 ) ) ;
#20386 = ORIENTED_EDGE ( 'NONE', *, *, #1080, .F. ) ;
#20388 = ORIENTED_EDGE ( 'NONE', *, *, #8234, .F. ) ;
#20389 = CARTESIAN_POINT ( 'NONE',  ( 0.3126073911696447549, 2.020725942163688504, 3.499999999999997780 ) ) ;
#20390 = ORIENTED_EDGE ( 'NONE', *, *, #8652, .T. ) ;
#20391 = ORIENTED_EDGE ( 'NONE', *, *, #6957, .T. ) ;
#20392 = DIRECTION ( 'NONE',  ( -1.000000000000000000, -2.699383410053119644E-30, -3.330669073875432643E-16 ) ) ;
#20393 = COLOUR_RGB ( '', 0.31764706, 0.68627451, 0.89019608) ;
#20394 = AXIS2_PLACEMENT_3D ( 'NONE', #21823, #22165, #6049 ) ;
#20395 = DIRECTION ( 'NONE',  ( 0.000000000000000000, 0.000000000000000000, 1.000000000000000000 ) ) ;
#20396 = CARTESIAN_POINT ( 'NONE',  ( -6.999999999999978684, -10.98142396999974046, 8.916666666666724694 ) ) ;
#20397 = VECTOR ( 'NONE', #19008, 1000.000000000000000 ) ;
#20398 = CARTESIAN_POINT ( 'NONE',  ( -89.70000000000064233, 4.857225732735059864E-14, -2.000000000000001776 ) ) ;
#20399 = CIRCLE ( 'NONE', #22649, 7.000000000000075495 ) ;
#20400 = DIRECTION ( 'NONE',  ( 2.013525853228507892E-32, 6.902532920683810383E-31, -1.000000000000000000 ) ) ;
#20401 = ADVANCED_FACE ( 'NONE', ( #15958 ), #21632, .T. ) ;
#20402 = VECTOR ( 'NONE', #14739, 1000.000000000000000 ) ;
#20403 = CARTESIAN_POINT ( 'NONE',  ( 54.42435809754109499, 2.499999999999946709, 6.500000000000144773 ) ) ;
#20404 = CARTESIAN_POINT ( 'NONE',  ( 7.000000000000001776, -3.018576030000261756, 8.916666666666687391 ) ) ;
#20405 = CARTESIAN_POINT ( 'NONE',  ( 3.950250160040463143, -0.7258013381037465850, 3.499999999999968914 ) ) ;
#20406 = DIRECTION ( 'NONE',  ( -2.220446049250313081E-16, 1.000000000000000000, -7.025792437124636392E-31 ) ) ;
#20407 = FACE_OUTER_BOUND ( 'NONE', #9216, .T. ) ;
#20408 = DIRECTION ( 'NONE',  ( -3.330669073875432643E-16, -4.437342591868153746E-31, 1.000000000000000000 ) ) ;
#20409 = FACE_OUTER_BOUND ( 'NONE', #22302, .T. ) ;
#20410 = CARTESIAN_POINT ( 'NONE',  ( -2.060000000000013820, 2.882395585961355661E-15, -0.3080913168122700885 ) ) ;
#20411 = ORIENTED_EDGE ( 'NONE', *, *, #5708, .T. ) ;
#20412 = CIRCLE ( 'NONE', #1991, 4.750000000000000888 ) ;
#20413 = FILL_AREA_STYLE ('',( #9241 ) ) ;
#20414 = AXIS2_PLACEMENT_3D ( 'NONE', #963, #20604, #8357 ) ;
#20416 = VERTEX_POINT ( 'NONE', #17978 ) ;
#20415 = ORIENTED_EDGE ( 'NONE', *, *, #19903, .F. ) ;
#20417 = AXIS2_PLACEMENT_3D ( 'NONE', #6105, #18679, #14805 ) ;
#20418 = CIRCLE ( 'NONE', #9148, 4.500000000000052403 ) ;
#20419 = AXIS2_PLACEMENT_3D ( 'NONE', #20515, #7800, #16494 ) ;
#20420 = ORIENTED_EDGE ( 'NONE', *, *, #19762, .T. ) ;
#20421 = EDGE_LOOP ( 'NONE', ( #1631, #15273, #14483, #7150 ) ) ;
#20422 = EDGE_LOOP ( 'NONE', ( #5340, #11777, #19490 ) ) ;
#20423 = VERTEX_POINT ( 'NONE', #19617 ) ;
#20424 = DIRECTION ( 'NONE',  ( 5.551115123561405253E-17, 1.000000000000000000, 2.256980353643891447E-27 ) ) ;
#20425 = CARTESIAN_POINT ( 'NONE',  ( 12.85000000000001386, -13.50000000000011191, -5.749999999999949374 ) ) ;
#20426 = ORIENTED_EDGE ( 'NONE', *, *, #3231, .T. ) ;
#20427 = CARTESIAN_POINT ( 'NONE',  ( -55.25320565519152893, 0.5000000000000905942, 8.000000000000035527 ) ) ;
#20428 = EDGE_CURVE ( 'NONE', #22215, #8787, #483, .T. ) ;
#20429 = AXIS2_PLACEMENT_3D ( 'NONE', #2574, #22573, #13637 ) ;
#20430 = CARTESIAN_POINT ( 'NONE',  ( 4.175813232069142344, 2.061359961916322980, 3.570380186727409200 ) ) ;
#20431 = AXIS2_PLACEMENT_3D ( 'NONE', #12170, #17585, #22457 ) ;
#20432 = CARTESIAN_POINT ( 'NONE',  ( 7.216878364870232154, 4.999999999999980460, 2.499999999999973355 ) ) ;
#20433 = DIRECTION ( 'NONE',  ( -2.172745813409349776E-17, 1.000000000000000000, -1.309377075419428048E-16 ) ) ;
#20434 = CIRCLE ( 'NONE', #16283, 2.500000000000002220 ) ;
#20435 = CARTESIAN_POINT ( 'NONE',  ( -7.971461718369612370, -11.76779483280641792, 7.625732677302382356 ) ) ;
#20436 = AXIS2_PLACEMENT_3D ( 'NONE', #3297, #17632, #10692 ) ;
#20437 = DIRECTION ( 'NONE',  ( 2.775557561562886729E-17, -4.401632478328199173E-16, 1.000000000000000000 ) ) ;
#20438 = LINE ( 'NONE', #15122, #6355 ) ;
#20439 = EDGE_CURVE ( 'NONE', #6969, #9218, #12555, .T. ) ;
#20440 = DIRECTION ( 'NONE',  ( -1.000000000000000000, -2.699383410053119644E-30, -3.330669073875432643E-16 ) ) ;
#20442 = EDGE_CURVE ( 'NONE', #13984, #10886, #19744, .T. ) ;
#20441 = DIRECTION ( 'NONE',  ( 3.032184104443272185E-30, 1.000000000000000000, -7.395570986447005381E-32 ) ) ;
#20443 = CARTESIAN_POINT ( 'NONE',  ( -2.678494666091062459, -3.072372537026391459, -0.03421028094655022972 ) ) ;
#20444 = CARTESIAN_POINT ( 'NONE',  ( 2.499999999999992006, 4.250000000000003553, -0.2500000000000349165 ) ) ;
#20445 = EDGE_LOOP ( 'NONE', ( #22792, #1212, #13437 ) ) ;
#20446 = CIRCLE ( 'NONE', #2775, 6.000000000000000000 ) ;
#20447 = ORIENTED_EDGE ( 'NONE', *, *, #20002, .F. ) ;
#20448 = AXIS2_PLACEMENT_3D ( 'NONE', #3677, #12487, #19684 ) ;
#20449 = EDGE_LOOP ( 'NONE', ( #4665, #2146, #15337, #22383 ) ) ;
#20450 = EDGE_LOOP ( 'NONE', ( #16749, #5383, #4705, #4629 ) ) ;
#20451 = CIRCLE ( 'NONE', #12172, 0.4999999999999990563 ) ;
#20452 = VERTEX_POINT ( 'NONE', #15839 ) ;
#20453 = CARTESIAN_POINT ( 'NONE',  ( -6.880723180993772785E-14, 4.999999999999976907, 4.749999999999958256 ) ) ;
#20454 = EDGE_CURVE ( 'NONE', #19937, #4283, #15733, .T. ) ;
#20455 = DIRECTION ( 'NONE',  ( 1.733449886265891589E-32, -4.190823558986610327E-31, 1.000000000000000000 ) ) ;
#20456 = ORIENTED_EDGE ( 'NONE', *, *, #4682, .T. ) ;
#20457 = CARTESIAN_POINT ( 'NONE',  ( 2.499999999999992006, 2.000000000000001776, -3.469446951953614189E-14 ) ) ;
#20458 = CARTESIAN_POINT ( 'NONE',  ( -2.742413778650615086, 1.750000000000001554, -4.750000000000004441 ) ) ;
#20459 = DIRECTION ( 'NONE',  ( -4.014645758689187542E-14, -6.938893903907237844E-15, -1.000000000000000000 ) ) ;
#20460 = EDGE_CURVE ( 'NONE', #19191, #16629, #1845, .T. ) ;
#20461 = DIRECTION ( 'NONE',  ( -1.000000000000000000, 5.319818659662146787E-14, -3.854941057726193231E-16 ) ) ;
#20462 = DIRECTION ( 'NONE',  ( -1.000000000000000000, -2.699383410053119644E-30, -3.330669073875432643E-16 ) ) ;
#20463 = DIRECTION ( 'NONE',  ( 0.000000000000000000, 0.000000000000000000, 1.000000000000000000 ) ) ;
#20464 = CARTESIAN_POINT ( 'NONE',  ( 6.000000000291855429, 2.999999999003851503, -5.999999999999998224 ) ) ;
#20465 = DIRECTION ( 'NONE',  ( -5.551115123561405253E-17, -1.000000000000000000, -2.256980353643891447E-27 ) ) ;
#20466 = CIRCLE ( 'NONE', #8810, 4.582731094065982447 ) ;
#20467 = FACE_OUTER_BOUND ( 'NONE', #2645, .T. ) ;
#20468 = EDGE_CURVE ( 'NONE', #22523, #8174, #1733, .T. ) ;
#20469 = CIRCLE ( 'NONE', #10313, 2.499999999999993783 ) ;
#20470 = VECTOR ( 'NONE', #20852, 1000.000000000000000 ) ;
#20471 = EDGE_CURVE ( 'NONE', #14576, #7345, #13862, .T. ) ;
#20472 = CARTESIAN_POINT ( 'NONE',  ( 3.880206590543188838, 3.396506438958500240, -1.117078279489074788 ) ) ;
#20473 = DIRECTION ( 'NONE',  ( 1.000000000000000000, 2.699383410053119644E-30, 3.330669073875432643E-16 ) ) ;
#20474 = AXIS2_PLACEMENT_3D ( 'NONE', #9000, #14633, #1920 ) ;
#20475 = EDGE_CURVE ( 'NONE', #16835, #21928, #13728, .T. ) ;
#20476 = LINE ( 'NONE', #11508, #13456 ) ;
#20477 = VERTEX_POINT ( 'NONE', #13966 ) ;
#20478 = ORIENTED_EDGE ( 'NONE', *, *, #11939, .F. ) ;
#20479 = ADVANCED_FACE ( 'NONE', ( #8917 ), #22744, .F. ) ;
#20480 = ADVANCED_FACE ( 'NONE', ( #17859 ), #16073, .T. ) ;
#20481 = EDGE_CURVE ( 'NONE', #6388, #7393, #18609, .T. ) ;
#20482 = EDGE_CURVE ( 'NONE', #2970, #11432, #5973, .T. ) ;
#20484 = ORIENTED_EDGE ( 'NONE', *, *, #8411, .T. ) ;
#20483 = ORIENTED_EDGE ( 'NONE', *, *, #17340, .F. ) ;
#20485 = DIRECTION ( 'NONE',  ( 1.000000000000000000, 4.440892098500626162E-16, -5.551115123125782702E-16 ) ) ;
#20486 = LINE ( 'NONE', #17161, #17862 ) ;
#20487 = DIRECTION ( 'NONE',  ( 1.000000000000000000, 0.000000000000000000, 0.000000000000000000 ) ) ;
#20488 = ORIENTED_EDGE ( 'NONE', *, *, #6241, .T. ) ;
#20489 = CARTESIAN_POINT ( 'NONE',  ( 4.175813232069149450, 4.122719923832687705, 1.040834085586084257E-14 ) ) ;
#20490 = ADVANCED_FACE ( 'NONE', ( #14549 ), #2197, .T. ) ;
#20491 = CARTESIAN_POINT ( 'NONE',  ( 6.000000000291855429, -0.5000000009961480529, -39.00000000000000000 ) ) ;
#20492 = CARTESIAN_POINT ( 'NONE',  ( 4.165266963751726337, -2.049631966911992897, 3.550066703508902854 ) ) ;
#20493 = CARTESIAN_POINT ( 'NONE',  ( -4.149603749300068145, 38.03274690132714397, -16.00313754524167109 ) ) ;
#20494 = FACE_OUTER_BOUND ( 'NONE', #18880, .T. ) ;
#20495 = EDGE_CURVE ( 'NONE', #1910, #7626, #14896, .T. ) ;
#20496 = B_SPLINE_CURVE_WITH_KNOTS ( 'NONE', 3,
 ( #21492, #1377, #1826, #14188, #14305, #10650, #8777, #23015, #12526, #5368, #9011, #12051, #13943, #19722, #8544, #1715 ),
 .UNSPECIFIED., .F., .F.,
 ( 4, 2, 2, 2, 2, 2, 2, 4 ),
 ( 0.000000000000000000, 0.0004262889904590540019, 0.0008525779809181080037, 0.001278866971377162114, 0.001705155961836216007, 0.002131444952295269684, 0.002557733942754324228, 0.003410311923672431147 ),
 .UNSPECIFIED. ) ;
#20497 = DIRECTION ( 'NONE',  ( 0.000000000000000000, 0.000000000000000000, -1.000000000000000000 ) ) ;
#20498 = CARTESIAN_POINT ( 'NONE',  ( -6.000000000000130562, 7.499999999999958256, -8.000000000000035527 ) ) ;
#20499 = DIRECTION ( 'NONE',  ( -4.190823558986625216E-31, 1.000000000000000000, -4.190823558986625216E-31 ) ) ;
#20500 = CARTESIAN_POINT ( 'NONE',  ( 81.85734743794770907, -6.246200939475254899, -6.499999999999970690 ) ) ;
#20501 = CARTESIAN_POINT ( 'NONE',  ( 4.330127018922110160, 4.689110867544560080, 7.499999999999985789 ) ) ;
#20502 = AXIS2_PLACEMENT_3D ( 'NONE', #9769, #20842, #6246 ) ;
#20503 = CARTESIAN_POINT ( 'NONE',  ( 66.26395429947832838, -7.000000000000006217, 6.000000000000172307 ) ) ;
#20504 = CARTESIAN_POINT ( 'NONE',  ( 0.3126073911696447549, -4.041451884327432076, 3.469446951953614189E-15 ) ) ;
#20505 = DIRECTION ( 'NONE',  ( -0.000000000000000000, 1.000000000000000000, -0.000000000000000000 ) ) ;
#20506 = ORIENTED_EDGE ( 'NONE', *, *, #6222, .T. ) ;
#20508 = ORIENTED_EDGE ( 'NONE', *, *, #14327, .T. ) ;
#20507 = ORIENTED_EDGE ( 'NONE', *, *, #9671, .F. ) ;
#20509 = VERTEX_POINT ( 'NONE', #5859 ) ;
#20510 = ORIENTED_EDGE ( 'NONE', *, *, #18177, .T. ) ;
#20512 = VERTEX_POINT ( 'NONE', #18318 ) ;
#20511 = ORIENTED_EDGE ( 'NONE', *, *, #14303, .T. ) ;
#20513 = AXIS2_PLACEMENT_3D ( 'NONE', #10354, #22959, #10133 ) ;
#20514 = ORIENTED_EDGE ( 'NONE', *, *, #7206, .T. ) ;
#20515 = CARTESIAN_POINT ( 'NONE',  ( 7.000000000000006217, -5.999999999999981348, 6.250000000000005329 ) ) ;
#20516 = CARTESIAN_POINT ( 'NONE',  ( 36.00000000029184832, 2.999999999003851503, -12.99999999999999822 ) ) ;
#20517 = ORIENTED_EDGE ( 'NONE', *, *, #4187, .F. ) ;
#20518 = CARTESIAN_POINT ( 'NONE',  ( 3.951447005078448260, 2.357513599190977249, 2.916666666666662078 ) ) ;
#20519 = FACE_OUTER_BOUND ( 'NONE', #15766, .T. ) ;
#20520 = LINE ( 'NONE', #14976, #889 ) ;
#20521 = LINE ( 'NONE', #15322, #20299 ) ;
#20522 = DIRECTION ( 'NONE',  ( 0.000000000000000000, 0.000000000000000000, -1.000000000000000000 ) ) ;
#20523 = DIRECTION ( 'NONE',  ( 0.8571428571428568732, 3.574076823648863958E-15, 0.5150787536377136044 ) ) ;
#20524 = DIRECTION ( 'NONE',  ( 0.000000000000000000, 0.000000000000000000, 1.000000000000000000 ) ) ;
#20525 = FACE_OUTER_BOUND ( 'NONE', #18002, .T. ) ;
#20526 = DIRECTION ( 'NONE',  ( 1.720845688168991849E-15, -1.000000000000000000, -6.656013887802284481E-31 ) ) ;
#20527 = EDGE_CURVE ( 'NONE', #23124, #19457, #14816, .T. ) ;
#20528 = PRESENTATION_LAYER_ASSIGNMENT (  '', '', ( #22773 ) ) ;
#20529 = DIRECTION ( 'NONE',  ( 3.885780586188016830E-16, 4.437342591868156373E-31, -1.000000000000000000 ) ) ;
#20530 = DIRECTION ( 'NONE',  ( 1.000000000000000000, 2.699383410053119644E-30, 3.330669073875432643E-16 ) ) ;
#20531 = CARTESIAN_POINT ( 'NONE',  ( -5.454524251050743899, 13.82936183575430356, -28.63121289012828186 ) ) ;
#20532 = DIRECTION ( 'NONE',  ( 1.000000000000000000, -1.424116703980815236E-16, -2.931272055834072749E-32 ) ) ;
#20533 = ORIENTED_EDGE ( 'NONE', *, *, #17582, .T. ) ;
#20535 = ORIENTED_EDGE ( 'NONE', *, *, #11533, .F. ) ;
#20534 = ORIENTED_EDGE ( 'NONE', *, *, #11070, .F. ) ;
#20536 = SHAPE_REPRESENTATION ( 'Hold Down Arm', ( #22115 ), #12708 ) ;
#20537 = VERTEX_POINT ( 'NONE', #3726 ) ;
#20538 = AXIS2_PLACEMENT_3D ( 'NONE', #5171, #12333, #3414 ) ;
#20539 = VERTEX_POINT ( 'NONE', #20088 ) ;
#20540 = ORIENTED_EDGE ( 'NONE', *, *, #3494, .T. ) ;
#20541 = AXIS2_PLACEMENT_3D ( 'NONE', #2785, #9842, #1029 ) ;
#20542 = VERTEX_POINT ( 'NONE', #14787 ) ;
#20543 = CARTESIAN_POINT ( 'NONE',  ( 3.951447005078447372, 3.704664227300100698, -0.5833333333333329263 ) ) ;
#20544 = FACE_OUTER_BOUND ( 'NONE', #21807, .T. ) ;
#20545 = ORIENTED_EDGE ( 'NONE', *, *, #5437, .T. ) ;
#20546 = DIRECTION ( 'NONE',  ( -0.000000000000000000, -1.000000000000000000, 0.000000000000000000 ) ) ;
#20547 = DIRECTION ( 'NONE',  ( 0.000000000000000000, 0.000000000000000000, 1.000000000000000000 ) ) ;
#20548 = DIRECTION ( 'NONE',  ( -1.000000000000000000, -6.224605580259554159E-31, 2.887593071917436153E-31 ) ) ;
#20549 = CARTESIAN_POINT ( 'NONE',  ( -8.518530740350131580, -11.95646899714138911, 6.984205661426534206 ) ) ;
#20550 = CARTESIAN_POINT ( 'NONE',  ( -6.999999999999978684, -5.999999999999981348, 11.74999999999998224 ) ) ;
#20551 = FACE_OUTER_BOUND ( 'NONE', #22854, .T. ) ;
#20552 = AXIS2_PLACEMENT_3D ( 'NONE', #15254, #4791, #19037 ) ;
#20553 = CARTESIAN_POINT ( 'NONE',  ( 37.60054931026106573, 0.05202134937407964371, -10.60054931026103553 ) ) ;
#20554 = AXIS2_PLACEMENT_3D ( 'NONE', #9092, #1905, #4131 ) ;
#20555 = SHAPE_REPRESENTATION_RELATIONSHIP ( 'NONE' , 'NONE' ,  #1856, #8352 ) ;
#20556 = CARTESIAN_POINT ( 'NONE',  ( 4.158806965674306078, 1.986429158307093212, 3.559403772175838476 ) ) ;
#20557 = DIRECTION ( 'NONE',  ( -1.000000000000000000, -3.254448077276381206E-32, -1.066788928082016908E-26 ) ) ;
#20559 = ORIENTED_EDGE ( 'NONE', *, *, #21633, .T. ) ;
#20558 = CONICAL_SURFACE ( 'NONE', #10406, 5.000000000000000888, 0.7853981633974430610 ) ;
#20560 = EDGE_CURVE ( 'NONE', #20996, #2526, #437, .T. ) ;
#20561 = VECTOR ( 'NONE', #21048, 1000.000000000000000 ) ;
#20562 = ORIENTED_EDGE ( 'NONE', *, *, #5085, .T. ) ;
#20563 = VERTEX_POINT ( 'NONE', #3836 ) ;
#20564 = ORIENTED_EDGE ( 'NONE', *, *, #17748, .T. ) ;
#20565 = PRODUCT ( 'Base', 'Base', '', ( #2236 ) ) ;
#20566 = ORIENTED_EDGE ( 'NONE', *, *, #1779, .F. ) ;
#20567 = FACE_BOUND ( 'NONE', #5462, .T. ) ;
#20568 = CARTESIAN_POINT ( 'NONE',  ( 12.84999999999997300, -1.999999999999998224, -2.549999999999997158 ) ) ;
#20569 = VERTEX_POINT ( 'NONE', #10896 ) ;
#20570 = AXIS2_PLACEMENT_3D ( 'NONE', #994, #4269, #17315 ) ;
#20571 = DIRECTION ( 'NONE',  ( 1.333893503340774882E-15, 2.778352770573747380E-17, 1.000000000000000000 ) ) ;
#20572 = AXIS2_PLACEMENT_3D ( 'NONE', #11842, #11714, #10306 ) ;
#20573 = FACE_BOUND ( 'NONE', #14051, .T. ) ;
#20574 = CARTESIAN_POINT ( 'NONE',  ( -65.47859922179029013, -6.938893903907228378E-14, -11.38422848940298593 ) ) ;
#20575 = CARTESIAN_POINT ( 'NONE',  ( 3.948103430090987853, 3.379418997638731881, 1.146674596025563320 ) ) ;
#20576 = AXIS2_PLACEMENT_3D ( 'NONE', #460, #14919, #9515 ) ;
#20577 = DIRECTION ( 'NONE',  ( 1.000000000000000000, 4.252453317207022018E-31, -5.551115123125818447E-17 ) ) ;
#20578 = CARTESIAN_POINT ( 'NONE',  ( -8.502135871254283828, -0.5075717384767730600, 6.995667647939113110 ) ) ;
#20579 = CYLINDRICAL_SURFACE ( 'NONE', #17860, 2.499999999999990674 ) ;
#20580 = CIRCLE ( 'NONE', #22459, 3.000000000000011546 ) ;
#20581 = CARTESIAN_POINT ( 'NONE',  ( 37.00000000000011369, 11.00000000000000000, -10.00000000000000888 ) ) ;
#20582 = DIRECTION ( 'NONE',  ( -1.000000000000000000, -2.699383410053119644E-30, -3.330669073875432643E-16 ) ) ;
#20583 = CARTESIAN_POINT ( 'NONE',  ( -95.20000000000065654, 6.938893903907228378E-15, 8.000000000000076383 ) ) ;
#20585 = AXIS2_PLACEMENT_3D ( 'NONE', #10159, #9933, #2636 ) ;
#20584 = CARTESIAN_POINT ( 'NONE',  ( -6.000000000000047073, -7.500000000000003553, 8.000000000000090594 ) ) ;
#20586 = EDGE_CURVE ( 'NONE', #3634, #11343, #7384, .T. ) ;
#20587 = CARTESIAN_POINT ( 'NONE',  ( 88.75737332930587797, -10.52760560296347947, -6.000000000000067502 ) ) ;
#20588 = CIRCLE ( 'NONE', #18329, 10.00000000000006395 ) ;
#20589 = VERTEX_POINT ( 'NONE', #7726 ) ;
#20590 = CIRCLE ( 'NONE', #6682, 0.4999999999999982236 ) ;
#20591 = EDGE_CURVE ( 'NONE', #14824, #19870, #15807, .T. ) ;
#20592 = EDGE_LOOP ( 'NONE', ( #19075, #4521, #2731, #21553 ) ) ;
#20593 = AXIS2_PLACEMENT_3D ( 'NONE', #9286, #12929, #2333 ) ;
#20594 = VECTOR ( 'NONE', #14478, 1000.000000000000000 ) ;
#20597 = ORIENTED_EDGE ( 'NONE', *, *, #4937, .F. ) ;
#20596 = EDGE_CURVE ( 'NONE', #16591, #20921, #18089, .T. ) ;
#20595 = EDGE_LOOP ( 'NONE', ( #15937, #14312, #19606, #5723 ) ) ;
#20598 = CIRCLE ( 'NONE', #312, 0.4999999999999978351 ) ;
#20599 = ADVANCED_FACE ( 'NONE', ( #13024 ), #11470, .T. ) ;
#20600 = CARTESIAN_POINT ( 'NONE',  ( 1.110223024625156540E-13, -1.750000000000001554, -4.750000000000000888 ) ) ;
#20601 = VERTEX_POINT ( 'NONE', #11832 ) ;
#20602 = DIRECTION ( 'NONE',  ( -0.9878135252003120703, -1.380506584136762427E-30, 0.1556420233463082226 ) ) ;
#20603 = DIRECTION ( 'NONE',  ( 3.885780586187836378E-16, 0.000000000000000000, -1.000000000000000000 ) ) ;
#20604 = DIRECTION ( 'NONE',  ( 2.172745813409349776E-17, -1.000000000000000000, 1.309377075419428048E-16 ) ) ;
#20605 = AXIS2_PLACEMENT_3D ( 'NONE', #9907, #17060, #20618 ) ;
#20606 = CARTESIAN_POINT ( 'NONE',  ( 4.175813232069142344, -2.061359961916371830, -3.570380186727398986 ) ) ;
#20607 = CARTESIAN_POINT ( 'NONE',  ( -6.938893903907228378E-14, -4.618802153517121312, -3.433295621305409107 ) ) ;
#20608 = CARTESIAN_POINT ( 'NONE',  ( -6.999999999999992006, -8.000000000000044409, 6.250000000000019540 ) ) ;
#20609 = CARTESIAN_POINT ( 'NONE',  ( -8.660254037844406838, 0.000000000000000000, 6.938893903907228378E-15 ) ) ;
#20610 = AXIS2_PLACEMENT_3D ( 'NONE', #23161, #19378, #21513 ) ;
#20611 = DIRECTION ( 'NONE',  ( 1.000000000000000000, 0.000000000000000000, 2.668805347656595124E-16 ) ) ;
#20612 = CARTESIAN_POINT ( 'NONE',  ( -4.690415759823418185, 0.7500000000000500711, -2.132253920548287773 ) ) ;
#20613 = ADVANCED_FACE ( 'NONE', ( #13605 ), #19197, .T. ) ;
#20614 = EDGE_CURVE ( 'NONE', #138, #9220, #17698, .T. ) ;
#20615 = VECTOR ( 'NONE', #6587, 1000.000000000000000 ) ;
#20616 = EDGE_CURVE ( 'NONE', #7096, #20801, #19267, .T. ) ;
#20617 = AXIS2_PLACEMENT_3D ( 'NONE', #17944, #5477, #19470 ) ;
#20618 = DIRECTION ( 'NONE',  ( 0.000000000000000000, 0.000000000000000000, 1.000000000000000000 ) ) ;
#20619 = CARTESIAN_POINT ( 'NONE',  ( 12.84999999999997300, -1.999999999999998224, 0.000000000000000000 ) ) ;
#20620 = ORIENTED_EDGE ( 'NONE', *, *, #9580, .T. ) ;
#20621 =( NAMED_UNIT ( * ) SI_UNIT ( $, .STERADIAN. ) SOLID_ANGLE_UNIT ( ) );
#20623 = ORIENTED_EDGE ( 'NONE', *, *, #1345, .T. ) ;
#20622 = ORIENTED_EDGE ( 'NONE', *, *, #11815, .T. ) ;
#20624 = EDGE_CURVE ( 'NONE', #10218, #7568, #5692, .T. ) ;
#20625 = PRESENTATION_LAYER_ASSIGNMENT (  '', '', ( #15720 ) ) ;
#20626 = ORIENTED_EDGE ( 'NONE', *, *, #19043, .F. ) ;
#20629 = VERTEX_POINT ( 'NONE', #22425 ) ;
#20628 = EDGE_CURVE ( 'NONE', #15636, #4169, #1549, .T. ) ;
#20627 = ORIENTED_EDGE ( 'NONE', *, *, #18691, .F. ) ;
#20630 = ADVANCED_FACE ( 'NONE', ( #7843 ), #21841, .T. ) ;
#20631 = DIRECTION ( 'NONE',  ( 1.000000000000000000, -4.437342591868175641E-31, 3.330669073875457788E-16 ) ) ;
#20632 = ORIENTED_EDGE ( 'NONE', *, *, #8889, .T. ) ;
#20633 = CARTESIAN_POINT ( 'NONE',  ( -3.999999999708153453, 13.99999999900385106, -19.50000000000000355 ) ) ;
#20634 = STYLED_ITEM ( 'NONE', ( #3777 ), #7961 ) ;
#20635 =( BOUNDED_SURFACE ( )  B_SPLINE_SURFACE ( 3, 2, ( 
 ( #11707, #22316, #8193 ),
 ( #13249, #16882, #7955 ),
 ( #911, #793, #6077 ),
 ( #15356, #16648, #20316 ),
 ( #18897, #11593, #4179 ),
 ( #22194, #22546, #11250 ),
 ( #15117, #1022, #6200 ),
 ( #6431, #20435, #20206 ),
 ( #11353, #22079, #4296 ),
 ( #4074, #13370, #9609 ),
 ( #15230, #18428, #18546 ),
 ( #2306, #20549, #4414 ),
 ( #562, #14895, #16760 ),
 ( #15008, #9839, #16990 ) ),
 .UNSPECIFIED., .F., .F., .T. ) 
 B_SPLINE_SURFACE_WITH_KNOTS ( ( 4, 2, 2, 2, 2, 2, 4 ),
 ( 3, 3 ),
 ( 2.168404344971008868E-19, 0.0009656398008937970437, 0.001448459701340695403, 0.001931279601787593871, 0.002414099502234492121, 0.002896919402681390806, 0.003862559203575187741 ),
 ( 0.000000000000000000, 1.000000000000000000 ),
 .UNSPECIFIED. ) 
 GEOMETRIC_REPRESENTATION_ITEM ( )  RATIONAL_B_SPLINE_SURFACE ( (
 ( 1.000000000000000000, 0.7071067811865499042, 1.000000000000000000),
 ( 1.000000000000000000, 0.6907538105665188555, 1.000000000000000000),
 ( 1.000000000000000000, 0.6765417438352628876, 1.000000000000000000),
 ( 1.000000000000000000, 0.6623232117677045894, 1.000000000000000000),
 ( 1.000000000000000000, 0.6588386061805797667, 1.000000000000000000),
 ( 1.000000000000000000, 0.6547992448372288443, 1.000000000000000000),
 ( 1.000000000000000000, 0.6542040191408818872, 1.000000000000000000),
 ( 1.000000000000000000, 0.6557724471762286234, 1.000000000000000000),
 ( 1.000000000000000000, 0.6579729115736443479, 1.000000000000000000),
 ( 1.000000000000000000, 0.6644691908065893937, 1.000000000000000000),
 ( 1.000000000000000000, 0.6687559023949966042, 1.000000000000000000),
 ( 1.000000000000000000, 0.6835702420292867343, 1.000000000000000000),
 ( 1.000000000000000000, 0.6960226107071281199, 1.000000000000000000),
 ( 1.000000000000000000, 0.7071067811865473507, 1.000000000000000000) ) ) 
 REPRESENTATION_ITEM ( '' )  SURFACE ( )  );
#20636 = AXIS2_PLACEMENT_3D ( 'NONE', #10074, #20675, #3136 ) ;
#20637 = DIRECTION ( 'NONE',  ( 1.000000000000000000, 2.220446049250314067E-16, -5.825996348268307008E-33 ) ) ;
#20638 = DIRECTION ( 'NONE',  ( -1.000000000000000000, 1.389842848855773367E-62, -2.013525853228507892E-32 ) ) ;
#20639 = CARTESIAN_POINT ( 'NONE',  ( -8.954763739086814667, -1.999999999999985567, 6.678571428571395963 ) ) ;
#20640 = FACE_OUTER_BOUND ( 'NONE', #23178, .T. ) ;
#20641 = CYLINDRICAL_SURFACE ( 'NONE', #16612, 2.999999999999999112 ) ;
#20642 = CARTESIAN_POINT ( 'NONE',  ( -45.56568542494959928, -2.108831175456959972, -8.000000000000035527 ) ) ;
#20643 = CARTESIAN_POINT ( 'NONE',  ( -4.000000000000100364, 2.309401076758546445, -3.433295621305381573 ) ) ;
#20644 = CARTESIAN_POINT ( 'NONE',  ( 37.68301270189235908, -1.703318040400119988E-14, -2.499999999999934275 ) ) ;
#20645 = MECHANICAL_DESIGN_GEOMETRIC_PRESENTATION_REPRESENTATION (  '', ( #11604 ), #12756 ) ;
#20646 = CARTESIAN_POINT ( 'NONE',  ( 116.8476484622116232, -8.074585193523331483, 6.500000000000040856 ) ) ;
#20647 = CYLINDRICAL_SURFACE ( 'NONE', #22492, 0.4999999999999987232 ) ;
#20648 = CARTESIAN_POINT ( 'NONE',  ( -6.230270079314315090, 13.95903802731504584, -28.01626849522005358 ) ) ;
#20649 = CARTESIAN_POINT ( 'NONE',  ( 3.972073812946706806, -0.6951863858493039228, -3.565770933504609719 ) ) ;
#20650 = ORIENTED_EDGE ( 'NONE', *, *, #17340, .T. ) ;
#20651 = PRODUCT_DEFINITION_CONTEXT ( 'detailed design', #15079, 'design' ) ;
#20652 =( GEOMETRIC_REPRESENTATION_CONTEXT ( 3 ) GLOBAL_UNCERTAINTY_ASSIGNED_CONTEXT ( ( #9097 ) ) GLOBAL_UNIT_ASSIGNED_CONTEXT ( ( #5214, #21455, #14495 ) ) REPRESENTATION_CONTEXT ( 'NONE', 'WORKASPACE' ) );
#20653 = SURFACE_SIDE_STYLE ('',( #6297 ) ) ;
#20655 = ORIENTED_EDGE ( 'NONE', *, *, #20624, .T. ) ;
#20654 = ORIENTED_EDGE ( 'NONE', *, *, #20586, .T. ) ;
#20656 = EDGE_CURVE ( 'NONE', #1880, #3212, #1190, .T. ) ;
#20657 = EDGE_LOOP ( 'NONE', ( #14462, #10213, #15043 ) ) ;
#20658 = ORIENTED_EDGE ( 'NONE', *, *, #7266, .T. ) ;
#20659 = MECHANICAL_DESIGN_GEOMETRIC_PRESENTATION_REPRESENTATION (  '', ( #18020 ), #3728 ) ;
#20660 = B_SPLINE_CURVE_WITH_KNOTS ( 'NONE', 3,
 ( #7239, #19229, #9003, #10753, #8882, #22891, #3247, #16155, #12276, #3127, #23250, #7135, #14295, #21480 ),
 .UNSPECIFIED., .F., .F.,
 ( 4, 2, 2, 2, 2, 2, 4 ),
 ( 0.000000000000000000, 0.0008249779604813624800, 0.001237466940722041064, 0.001649955920962719756, 0.002062444901203395412, 0.002474933881444070418, 0.003299911841925418261 ),
 .UNSPECIFIED. ) ;
#20661 = ORIENTED_EDGE ( 'NONE', *, *, #950, .T. ) ;
#20662 = EDGE_CURVE ( 'NONE', #5983, #1520, #18081, .T. ) ;
#20663 = EDGE_LOOP ( 'NONE', ( #7998, #5045, #19661, #5812 ) ) ;
#20664 = DIRECTION ( 'NONE',  ( -1.000000000000000000, -1.479114197289397135E-31, -5.916456789157588541E-31 ) ) ;
#20665 = DIRECTION ( 'NONE',  ( -0.8122328620674128530, 0.000000000000000000, -0.5833333333333344806 ) ) ;
#20666 = VERTEX_POINT ( 'NONE', #6553 ) ;
#20667 = DIRECTION ( 'NONE',  ( 1.374679200952785197E-16, 1.000000000000000000, 0.000000000000000000 ) ) ;
#20668 = DIRECTION ( 'NONE',  ( 1.454462294001240516E-30, 1.000000000000000000, 7.888609052210128564E-31 ) ) ;
#20669 = DIRECTION ( 'NONE',  ( 1.000000000000000000, 0.000000000000000000, 0.000000000000000000 ) ) ;
#20670 = DIRECTION ( 'NONE',  ( 0.000000000000000000, -0.000000000000000000, -1.000000000000000000 ) ) ;
#20671 = CARTESIAN_POINT ( 'NONE',  ( 27.99999999999991118, -3.469446951953614189E-15, 2.499999999999962697 ) ) ;
#20672 = CARTESIAN_POINT ( 'NONE',  ( 4.151274195509686571, 4.079825909417490237, -1.471199427103728571E-15 ) ) ;
#20673 = MANIFOLD_SOLID_BREP ( 'EndChamfer', #12936 ) ;
#20674 = CARTESIAN_POINT ( 'NONE',  ( -7.345446946324452497, -13.78184793132693642, 7.860330092054036655 ) ) ;
#20675 = DIRECTION ( 'NONE',  ( 2.220446049250314067E-16, -1.000000000000000000, 7.025792437124636392E-31 ) ) ;
#20676 = AXIS2_PLACEMENT_3D ( 'NONE', #12755, #20054, #5933 ) ;
#20677 = DIRECTION ( 'NONE',  ( -1.333893503340774882E-15, -2.778352770573747380E-17, -1.000000000000000000 ) ) ;
#20678 = CARTESIAN_POINT ( 'NONE',  ( -4.749999999999985789, 3.766740792898615283E-14, -1.500000000000001332 ) ) ;
#20679 = ORIENTED_EDGE ( 'NONE', *, *, #22725, .F. ) ;
#20680 = ORIENTED_EDGE ( 'NONE', *, *, #22146, .T. ) ;
#20681 = CARTESIAN_POINT ( 'NONE',  ( 42.00000000000014921, 11.00000000000000000, -6.499999999999950262 ) ) ;
#20682 = FACE_BOUND ( 'NONE', #17870, .T. ) ;
#20683 = VERTEX_POINT ( 'NONE', #19358 ) ;
#20684 = VERTEX_POINT ( 'NONE', #23138 ) ;
#20685 = ORIENTED_EDGE ( 'NONE', *, *, #3646, .T. ) ;
#20686 = EDGE_LOOP ( 'NONE', ( #21585, #18120, #15221, #2612, #11845, #11816 ) ) ;
#20687 = CARTESIAN_POINT ( 'NONE',  ( -4.000000000000003553, 1.557668341133521483, -5.440303434304241570 ) ) ;
#20688 = LINE ( 'NONE', #20568, #13297 ) ;
#20689 = ORIENTED_EDGE ( 'NONE', *, *, #20792, .F. ) ;
#20690 = VECTOR ( 'NONE', #3670, 1000.000000000000000 ) ;
#20691 = DIRECTION ( 'NONE',  ( -1.066786462891689527E-26, -6.656013887802287108E-31, -1.000000000000000000 ) ) ;
#20692 = LINE ( 'NONE', #8452, #17527 ) ;
#20693 = LINE ( 'NONE', #15148, #14343 ) ;
#20694 = CARTESIAN_POINT ( 'NONE',  ( 54.42435809754109499, 2.999999999999947153, 6.500000000000144773 ) ) ;
#20695 = CARTESIAN_POINT ( 'NONE',  ( 7.596194078004423034, 47.59619407671642222, -26.50000000000000000 ) ) ;
#20696 = FACE_OUTER_BOUND ( 'NONE', #400, .T. ) ;
#20697 = DIRECTION ( 'NONE',  ( 7.543342432310246422E-27, 0.7071067811865516806, 0.7071067811865434649 ) ) ;
#20698 = EDGE_CURVE ( 'NONE', #11721, #15489, #14331, .T. ) ;
#20699 = CARTESIAN_POINT ( 'NONE',  ( 12.49999999999992362, 1.250000000000015099, -9.500000000000001776 ) ) ;
#20700 = DIRECTION ( 'NONE',  ( -0.000000000000000000, -1.000000000000000000, 0.000000000000000000 ) ) ;
#20701 = PLANE ( 'NONE',  #9896 ) ;
#20702 = DIRECTION ( 'NONE',  ( -1.000000000000000000, 4.190823558986610327E-31, -1.733449886265890494E-32 ) ) ;
#20703 = PLANE ( 'NONE',  #16370 ) ;
#20704 = CARTESIAN_POINT ( 'NONE',  ( -2.250000000000001776, 2.879267452445610575E-14, 17.49999999999997513 ) ) ;
#20705 = CIRCLE ( 'NONE', #18069, 4.500000000000000888 ) ;
#20706 = ORIENTED_EDGE ( 'NONE', *, *, #883, .F. ) ;
#20707 = ITEM_DEFINED_TRANSFORMATION ( 'NONE', 'NONE', #12771,  #22115 ) ;
#20708 = ORIENTED_EDGE ( 'NONE', *, *, #5574, .T. ) ;
#20710 = ORIENTED_EDGE ( 'NONE', *, *, #17744, .T. ) ;
#20709 = ORIENTED_EDGE ( 'NONE', *, *, #22981, .F. ) ;
#20711 = ORIENTED_EDGE ( 'NONE', *, *, #4473, .T. ) ;
#20712 = CARTESIAN_POINT ( 'NONE',  ( 0.000000000000000000, 0.000000000000000000, 0.000000000000000000 ) ) ;
#20713 = DIRECTION ( 'NONE',  ( 7.395570986446975166E-31, 3.382522293539642133E-32, 1.000000000000000000 ) ) ;
#20714 = DIRECTION ( 'NONE',  ( 1.000000000000000000, 3.254448077276381206E-32, 1.066788928082016908E-26 ) ) ;
#20715 = ORIENTED_EDGE ( 'NONE', *, *, #14362, .F. ) ;
#20716 = VECTOR ( 'NONE', #14580, 1000.000000000000000 ) ;
#20717 = AXIS2_PLACEMENT_3D ( 'NONE', #7164, #14322, #19263 ) ;
#20718 = CARTESIAN_POINT ( 'NONE',  ( -50.65685424949274562, 3.200000000000022382, -8.000000000000062172 ) ) ;
#20719 = LINE ( 'NONE', #2834, #9428 ) ;
#20720 = DIRECTION ( 'NONE',  ( 0.000000000000000000, 0.000000000000000000, 1.000000000000000000 ) ) ;
#20721 = ADVANCED_FACE ( 'NONE', ( #15812 ), #6894, .T. ) ;
#20722 = CARTESIAN_POINT ( 'NONE',  ( -12.84999999999999964, -13.50000000000011191, -5.749999999999949374 ) ) ;
#20723 = LINE ( 'NONE', #12106, #15189 ) ;
#20724 = CARTESIAN_POINT ( 'NONE',  ( -42.54314575050782565, -7.500000000000038192, -8.000000000000007105 ) ) ;
#20725 = CARTESIAN_POINT ( 'NONE',  ( -1.400962679198869567E-14, -24.99999999999998224, -4.750000000000013323 ) ) ;
#20726 = DIRECTION ( 'NONE',  ( 1.734723475976805517E-15, 1.000000000000000000, 0.000000000000000000 ) ) ;
#20727 = DIRECTION ( 'NONE',  ( -1.000000000000000000, -6.224605580259554159E-31, 2.887593071917436153E-31 ) ) ;
#20728 = EDGE_CURVE ( 'NONE', #4887, #9452, #10921, .T. ) ;
#20729 = LINE ( 'NONE', #19305, #2547 ) ;
#20730 = ADVANCED_FACE ( 'NONE', ( #10532 ), #8433, .F. ) ;
#20731 = DIRECTION ( 'NONE',  ( -1.000000000000000000, 3.552713678800500929E-15, 0.000000000000000000 ) ) ;
#20732 = CARTESIAN_POINT ( 'NONE',  ( 6.999999999999978684, -8.000000000000031974, 10.24999999999998224 ) ) ;
#20733 = EDGE_CURVE ( 'NONE', #3527, #7132, #10181, .T. ) ;
#20734 = ORIENTED_EDGE ( 'NONE', *, *, #6967, .T. ) ;
#20735 =( LENGTH_UNIT ( ) NAMED_UNIT ( * ) SI_UNIT ( .MILLI., .METRE. ) );
#20736 = AXIS2_PLACEMENT_3D ( 'NONE', #2365, #5802, #9318 ) ;
#20737 = AXIS2_PLACEMENT_3D ( 'NONE', #5760, #19550, #21092 ) ;
#20739 = ORIENTED_EDGE ( 'NONE', *, *, #19481, .T. ) ;
#20738 = ORIENTED_EDGE ( 'NONE', *, *, #9103, .T. ) ;
#20740 = ORIENTED_EDGE ( 'NONE', *, *, #18018, .T. ) ;
#20742 = EDGE_LOOP ( 'NONE', ( #8313, #19840, #4459, #1518 ) ) ;
#20741 = VERTEX_POINT ( 'NONE', #22780 ) ;
#20743 = B_SPLINE_CURVE_WITH_KNOTS ( 'NONE', 3,
 ( #22989, #17446, #53, #18154 ),
 .UNSPECIFIED., .F., .F.,
 ( 4, 4 ),
 ( 2.309401076744506391E-07, 0.004330357959029864159 ),
 .UNSPECIFIED. ) ;
#20744 = CARTESIAN_POINT ( 'NONE',  ( -4.000000000000003553, 2.309401076758494487, -0.3572655899081629283 ) ) ;
#20745 = FACE_OUTER_BOUND ( 'NONE', #374, .T. ) ;
#20746 = ADVANCED_FACE ( 'NONE', ( #15700 ), #22899, .T. ) ;
#20747 = LINE ( 'NONE', #21091, #15534 ) ;
#20748 = EDGE_CURVE ( 'NONE', #6130, #15653, #12284, .T. ) ;
#20749 = CARTESIAN_POINT ( 'NONE',  ( 2.775557561562891351E-14, 8.000000000000003553, -12.99999999999999822 ) ) ;
#20750 = DIRECTION ( 'NONE',  ( 1.000000000000000000, -4.190823558986621713E-31, 0.000000000000000000 ) ) ;
#20751 = VECTOR ( 'NONE', #7585, 1000.000000000000000 ) ;
#20752 = CARTESIAN_POINT ( 'NONE',  ( -7.324400034341836729, -2.232976452217596997, 7.601326208249630234 ) ) ;
#20753 = EDGE_CURVE ( 'NONE', #15346, #235, #21087, .T. ) ;
#20754 = CYLINDRICAL_SURFACE ( 'NONE', #13697, 4.000000000000045297 ) ;
#20755 = DIRECTION ( 'NONE',  ( 1.000000000000000000, 0.000000000000000000, 0.000000000000000000 ) ) ;
#20756 = CARTESIAN_POINT ( 'NONE',  ( 7.263517083688649123, -2.279413854694211761, 7.724990489865469989 ) ) ;
#20757 = CIRCLE ( 'NONE', #1578, 4.000000000000045297 ) ;
#20758 = AXIS2_PLACEMENT_3D ( 'NONE', #1614, #1949, #9140 ) ;
#20759 = CARTESIAN_POINT ( 'NONE',  ( 4.180345472528539830, 2.086001522971435040, 3.570468649087209290 ) ) ;
#20760 = CYLINDRICAL_SURFACE ( 'NONE', #16600, 0.5000000000000004441 ) ;
#20761 = AXIS2_PLACEMENT_3D ( 'NONE', #7271, #14087, #7159 ) ;
#20762 = CARTESIAN_POINT ( 'NONE',  ( 0.000000000000000000, -3.031088913245536087, 1.750000000000003331 ) ) ;
#20763 = ADVANCED_FACE ( 'NONE', ( #6259 ), #16705, .F. ) ;
#20764 = FACE_OUTER_BOUND ( 'NONE', #18466, .T. ) ;
#20765 = DIRECTION ( 'NONE',  ( 3.885780586188016830E-16, 4.437342591868156373E-31, -1.000000000000000000 ) ) ;
#20766 = DIRECTION ( 'NONE',  ( 1.333893503340774882E-15, 2.778352770573747380E-17, 1.000000000000000000 ) ) ;
#20767 = PRODUCT_DEFINITION_SHAPE ( 'NONE', 'NONE',  #11778 ) ;
#20768 = EDGE_CURVE ( 'NONE', #13336, #19280, #388, .T. ) ;
#20769 = ORIENTED_EDGE ( 'NONE', *, *, #9253, .T. ) ;
#20771 = EDGE_LOOP ( 'NONE', ( #4754, #18362, #10624, #13883 ) ) ;
#20770 = ORIENTED_EDGE ( 'NONE', *, *, #10957, .T. ) ;
#20772 = ORIENTED_EDGE ( 'NONE', *, *, #22021, .T. ) ;
#20773 = ORIENTED_EDGE ( 'NONE', *, *, #8562, .F. ) ;
#20774 = PRESENTATION_LAYER_ASSIGNMENT (  '', '', ( #7610 ) ) ;
#20775 = AXIS2_PLACEMENT_3D ( 'NONE', #19469, #23131, #10638 ) ;
#20776 = VERTEX_POINT ( 'NONE', #7778 ) ;
#20777 = AXIS2_PLACEMENT_3D ( 'NONE', #4555, #4315, #7977 ) ;
#20778 = AXIS2_PLACEMENT_3D ( 'NONE', #20898, #2888, #6427 ) ;
#20779 = EDGE_CURVE ( 'NONE', #19367, #12208, #5316, .T. ) ;
#20780 = AXIS2_PLACEMENT_3D ( 'NONE', #4256, #16726, #5702 ) ;
#20781 = ORIENTED_EDGE ( 'NONE', *, *, #2773, .F. ) ;
#20782 = PLANE ( 'NONE',  #17051 ) ;
#20783 = ADVANCED_FACE ( 'NONE', ( #4014 ), #4127, .F. ) ;
#20784 = CARTESIAN_POINT ( 'NONE',  ( 0.000000000000000000, 0.000000000000000000, 0.000000000000000000 ) ) ;
#20785 = ORIENTED_EDGE ( 'NONE', *, *, #8539, .T. ) ;
#20786 = CARTESIAN_POINT ( 'NONE',  ( 1.369266385878522785, -4.353985157227390831E-16, 4.607329295533711289 ) ) ;
#20787 = CYLINDRICAL_SURFACE ( 'NONE', #15123, 2.500000000000015543 ) ;
#20788 = FACE_OUTER_BOUND ( 'NONE', #6305, .T. ) ;
#20789 = CARTESIAN_POINT ( 'NONE',  ( 42.50000000000020606, 8.000000000000003553, -13.00000000000002487 ) ) ;
#20790 = B_SPLINE_CURVE_WITH_KNOTS ( 'NONE', 3,
 ( #3440, #14492, #17909, #6986, #5556, #3561, #18029, #19788, #18251, #1784, #10942, #3774, #2010, #41 ),
 .UNSPECIFIED., .F., .F.,
 ( 4, 2, 2, 2, 2, 2, 4 ),
 ( 0.000000000000000000, 0.0004465115319127595738, 0.0008930230638255191476, 0.001339534595738282570, 0.001786046127651045885, 0.002679069191476572079, 0.003572092255302097407 ),
 .UNSPECIFIED. ) ;
#20791 = FACE_OUTER_BOUND ( 'NONE', #8966, .T. ) ;
#20792 = EDGE_CURVE ( 'NONE', #10595, #235, #9555, .T. ) ;
#20793 = DIRECTION ( 'NONE',  ( -1.000000000000000000, 7.100545512326564696E-57, 1.066786462891689527E-26 ) ) ;
#20794 = CARTESIAN_POINT ( 'NONE',  ( -7.991520206789724412, -13.39565235458639059, 7.599114430427917455 ) ) ;
#20795 = DIRECTION ( 'NONE',  ( 1.000000000000000000, -4.190823558986610327E-31, 1.733449886265890494E-32 ) ) ;
#20796 = AXIS2_PLACEMENT_3D ( 'NONE', #5091, #21679, #8973 ) ;
#20797 = DIRECTION ( 'NONE',  ( 0.000000000000000000, 0.000000000000000000, -1.000000000000000000 ) ) ;
#20798 = VECTOR ( 'NONE', #15110, 1000.000000000000000 ) ;
#20799 = LINE ( 'NONE', #11711, #11892 ) ;
#20800 = VECTOR ( 'NONE', #5801, 1000.000000000000114 ) ;
#20801 = VERTEX_POINT ( 'NONE', #16583 ) ;
#20802 = VECTOR ( 'NONE', #6394, 1000.000000000000000 ) ;
#20803 = SURFACE_STYLE_USAGE ( .BOTH. , #22553 ) ;
#20804 = DIRECTION ( 'NONE',  ( -1.000000000000000000, -3.254448077276381206E-32, -1.066788928082016908E-26 ) ) ;
#20805 = DIRECTION ( 'NONE',  ( -9.121204216617949000E-31, -1.000000000000000000, 6.982962677686261977E-15 ) ) ;
#20806 = EDGE_LOOP ( 'NONE', ( #5083, #16372, #425, #7736 ) ) ;
#20807 = ORIENTED_EDGE ( 'NONE', *, *, #7649, .F. ) ;
#20808 = ORIENTED_EDGE ( 'NONE', *, *, #913, .F. ) ;
#20809 = EDGE_LOOP ( 'NONE', ( #10398, #9569, #13330 ) ) ;
#20810 = DIRECTION ( 'NONE',  ( 0.000000000000000000, 7.806255641895571971E-15, 1.000000000000000000 ) ) ;
#20811 = FACE_OUTER_BOUND ( 'NONE', #2875, .T. ) ;
#20812 = VECTOR ( 'NONE', #3046, 1000.000000000000000 ) ;
#20813 = ORIENTED_EDGE ( 'NONE', *, *, #3221, .F. ) ;
#20814 = VECTOR ( 'NONE', #13395, 1000.000000000000000 ) ;
#20815 = CARTESIAN_POINT ( 'NONE',  ( -43.10883117545714782, -5.300000000000020250, 7.500000000000062172 ) ) ;
#20816 = AXIS2_PLACEMENT_3D ( 'NONE', #11273, #457, #20461 ) ;
#20817 = AXIS2_PLACEMENT_3D ( 'NONE', #1500, #21271, #3611 ) ;
#20818 = DIRECTION ( 'NONE',  ( 1.000000000000000000, -4.190823558986610327E-31, 1.733449886265890494E-32 ) ) ;
#20819 = LINE ( 'NONE', #6575, #16221 ) ;
#20821 = EDGE_CURVE ( 'NONE', #20563, #16003, #11310, .T. ) ;
#20820 = COLOUR_RGB ( '', 0.40784314, 0.44705882, 0.49803922) ;
#20822 = DIRECTION ( 'NONE',  ( -1.000000000000000000, -2.699383410053119644E-30, -3.330669073875432643E-16 ) ) ;
#20823 = DIRECTION ( 'NONE',  ( -9.121204216617949000E-31, -1.000000000000000000, 6.982962677686261977E-15 ) ) ;
#20824 =( REPRESENTATION_RELATIONSHIP ('NONE','NONE', #19450, #15574 ) REPRESENTATION_RELATIONSHIP_WITH_TRANSFORMATION ( #29 )SHAPE_REPRESENTATION_RELATIONSHIP( ) );
#20825 = CARTESIAN_POINT ( 'NONE',  ( -7.694134585029414275, -0.3119908745746264866, 8.172315317061135787 ) ) ;
#20826 = ADVANCED_FACE ( 'NONE', ( #616, #20265 ), #7899, .F. ) ;
#20827 = CARTESIAN_POINT ( 'NONE',  ( 8.721922330812452273, -13.98762810781384403, 6.818491697977837163 ) ) ;
#20828 = CARTESIAN_POINT ( 'NONE',  ( -64.00000000000045475, -0.5000000000000628386, -2.000000000000001776 ) ) ;
#20829 = CARTESIAN_POINT ( 'NONE',  ( 24.74999999999997158, 1.999999999999988010, -18.74999999999998224 ) ) ;
#20830 = DIRECTION ( 'NONE',  ( 0.000000000000000000, 0.000000000000000000, 1.000000000000000000 ) ) ;
#20831 = DIRECTION ( 'NONE',  ( 1.000000000000000000, -1.389842848855773367E-62, 2.013525853228507892E-32 ) ) ;
#20832 = EDGE_CURVE ( 'NONE', #4468, #17822, #503, .T. ) ;
#20833 = AXIS2_PLACEMENT_3D ( 'NONE', #10535, #17592, #14304 ) ;
#20834 = CARTESIAN_POINT ( 'NONE',  ( 2.918498775983380256E-10, 2.999999999003851503, -26.00000000000000000 ) ) ;
#20835 = AXIS2_PLACEMENT_3D ( 'NONE', #5803, #5904, #7670 ) ;
#20836 = MANIFOLD_SOLID_BREP ( 'Fillet1', #552 ) ;
#20837 = VERTEX_POINT ( 'NONE', #13318 ) ;
#20839 = EDGE_LOOP ( 'NONE', ( #19216, #8788, #9912 ) ) ;
#20838 = ORIENTED_EDGE ( 'NONE', *, *, #766, .F. ) ;
#20840 = ORIENTED_EDGE ( 'NONE', *, *, #4318, .T. ) ;
#20841 = DIRECTION ( 'NONE',  ( 1.613696256722611405E-16, -0.000000000000000000, 1.000000000000000000 ) ) ;
#20842 = DIRECTION ( 'NONE',  ( 5.551115123125782702E-16, 2.146163712481653435E-16, -1.000000000000000000 ) ) ;
#20843 = DIRECTION ( 'NONE',  ( 0.000000000000000000, 0.000000000000000000, -1.000000000000000000 ) ) ;
#20844 = AXIS2_PLACEMENT_3D ( 'NONE', #13571, #8619, #11673 ) ;
#20845 = ORIENTED_EDGE ( 'NONE', *, *, #11027, .F. ) ;
#20846 = VECTOR ( 'NONE', #8017, 1000.000000000000000 ) ;
#20847 = LINE ( 'NONE', #1309, #18371 ) ;
#20848 = CARTESIAN_POINT ( 'NONE',  ( -3.999999999708153453, 13.99999999900385106, -19.50000000000000355 ) ) ;
#20849 = AXIS2_PLACEMENT_3D ( 'NONE', #3243, #8642, #15686 ) ;
#20850 = CARTESIAN_POINT ( 'NONE',  ( -2.742413778650712342, 1.325747111984031834, 4.749999999999999112 ) ) ;
#20851 = DIRECTION ( 'NONE',  ( -1.000000000000000000, 0.000000000000000000, 0.000000000000000000 ) ) ;
#20852 = DIRECTION ( 'NONE',  ( 2.172745813409349776E-17, -1.000000000000000000, 1.309377075419428048E-16 ) ) ;
#20853 = DIRECTION ( 'NONE',  ( -2.753132232808523448E-17, 0.6666666666666727359, 0.7453559924999245689 ) ) ;
#20854 = CARTESIAN_POINT ( 'NONE',  ( 2.775557561562891351E-14, 8.000000000000003553, -12.50000000000001066 ) ) ;
#20855 = DIRECTION ( 'NONE',  ( 0.6819983600624998088, 0.7313537016191693496, 0.000000000000000000 ) ) ;
#20856 = DIRECTION ( 'NONE',  ( 1.000000000000000000, 3.254448077276381206E-32, 1.066788928082016908E-26 ) ) ;
#20857 = ORIENTED_EDGE ( 'NONE', *, *, #11239, .F. ) ;
#20858 = PRODUCT_DEFINITION ( 'UNKNOWN', '', #16133, #9125 ) ;
#20860 = VERTEX_POINT ( 'NONE', #20500 ) ;
#20859 = ORIENTED_EDGE ( 'NONE', *, *, #11022, .F. ) ;
#20861 = ADVANCED_FACE ( 'NONE', ( #846 ), #18485, .T. ) ;
#20862 = ORIENTED_EDGE ( 'NONE', *, *, #8067, .F. ) ;
#20864 = ORIENTED_EDGE ( 'NONE', *, *, #17919, .F. ) ;
#20863 = ORIENTED_EDGE ( 'NONE', *, *, #20987, .T. ) ;
#20865 = DIRECTION ( 'NONE',  ( -0.7313537016191752338, 0.6819983600624933695, 1.628001950178161200E-16 ) ) ;
#20866 = DIRECTION ( 'NONE',  ( 0.000000000000000000, 0.000000000000000000, 1.000000000000000000 ) ) ;
#20867 = CARTESIAN_POINT ( 'NONE',  ( -65.00000000000046896, -6.245004513516505540E-14, 3.000000000000030198 ) ) ;
#20868 = DIRECTION ( 'NONE',  ( 1.000000000000000000, 0.000000000000000000, 0.000000000000000000 ) ) ;
#20869 = DIRECTION ( 'NONE',  ( -7.860214984770699307E-18, 1.409037165336591006E-16, 1.000000000000000000 ) ) ;
#20870 = CARTESIAN_POINT ( 'NONE',  ( -7.971461718369176275, -2.232205167193757056, 7.625732677302567986 ) ) ;
#20871 = CIRCLE ( 'NONE', #10711, 6.500000000000067502 ) ;
#20872 = FACE_OUTER_BOUND ( 'NONE', #4750, .T. ) ;
#20873 = CARTESIAN_POINT ( 'NONE',  ( 119.5756419024614132, 0.5000000000000004441, -6.499999999999964473 ) ) ;
#20874 = CARTESIAN_POINT ( 'NONE',  ( 4.030875481281778860, 1.403567514398415206, 3.499999999999996003 ) ) ;
#20875 = DIRECTION ( 'NONE',  ( 6.938893903907224433E-16, -3.552713678800500929E-15, -1.000000000000000000 ) ) ;
#20876 = CARTESIAN_POINT ( 'NONE',  ( -55.05572809000130974, 0.5000000000000143219, -8.000000000000035527 ) ) ;
#20877 = DIRECTION ( 'NONE',  ( 1.000000000000000000, 0.000000000000000000, 0.000000000000000000 ) ) ;
#20878 = CARTESIAN_POINT ( 'NONE',  ( -2.296348136152782882, 1.454515171370275084, -4.750000000000025757 ) ) ;
#20879 = CARTESIAN_POINT ( 'NONE',  ( 3.961545574370236800, 1.423222908132905307, -3.500000000000006217 ) ) ;
#20880 = VERTEX_POINT ( 'NONE', #1822 ) ;
#20881 = PRODUCT_DEFINITION_CONTEXT ( 'detailed design', #18699, 'design' ) ;
#20882 = EDGE_CURVE ( 'NONE', #13641, #4111, #3283, .T. ) ;
#20884 = VERTEX_POINT ( 'NONE', #17058 ) ;
#20883 = ORIENTED_EDGE ( 'NONE', *, *, #17284, .T. ) ;
#20885 = EDGE_CURVE ( 'NONE', #10125, #19105, #11160, .T. ) ;
#20886 = ORIENTED_EDGE ( 'NONE', *, *, #16840, .F. ) ;
#20887 = ORIENTED_EDGE ( 'NONE', *, *, #12856, .T. ) ;
#20888 = ORIENTED_EDGE ( 'NONE', *, *, #4784, .T. ) ;
#20889 = CARTESIAN_POINT ( 'NONE',  ( 4.175572532730924991, -2.061029303918041400, 3.569807470274398487 ) ) ;
#20890 = EDGE_CURVE ( 'NONE', #4029, #5959, #12945, .T. ) ;
#20891 = EDGE_CURVE ( 'NONE', #11432, #3321, #2525, .T. ) ;
#20892 = DIRECTION ( 'NONE',  ( 0.000000000000000000, -7.888609052210128564E-31, 1.000000000000000000 ) ) ;
#20893 = ORIENTED_EDGE ( 'NONE', *, *, #17828, .F. ) ;
#20894 = DIRECTION ( 'NONE',  ( 1.000000000000000000, -4.440892098500654758E-16, 0.000000000000000000 ) ) ;
#20895 = ADVANCED_FACE ( 'NONE', ( #2841 ), #13666, .F. ) ;
#20896 = CARTESIAN_POINT ( 'NONE',  ( 3.673643420401899728, 2.497823135841254150, -5.351519936625005691 ) ) ;
#20897 = VECTOR ( 'NONE', #13403, 1000.000000000000000 ) ;
#20898 = CARTESIAN_POINT ( 'NONE',  ( 3.000000000291852764, 42.99999999900385461, -29.00000000000000355 ) ) ;
#20899 = DIRECTION ( 'NONE',  ( -1.000000000000000000, 0.000000000000000000, -3.717264591378832268E-16 ) ) ;
#20900 = CARTESIAN_POINT ( 'NONE',  ( -6.938893903907228378E-14, 4.999999999999976907, -4.163336342344337027E-14 ) ) ;
#20901 = DIRECTION ( 'NONE',  ( 7.395570986446975166E-31, 3.382522293539642133E-32, 1.000000000000000000 ) ) ;
#20902 = FILL_AREA_STYLE_COLOUR ( '', #22590 ) ;
#20903 = FACE_OUTER_BOUND ( 'NONE', #4282, .T. ) ;
#20904 = LINE ( 'NONE', #6898, #17421 ) ;
#20905 = CARTESIAN_POINT ( 'NONE',  ( 37.29045043747289156, 0.08880391167994089452, -10.57823792062843715 ) ) ;
#20906 = EDGE_CURVE ( 'NONE', #14484, #1201, #9664, .T. ) ;
#20907 = EDGE_LOOP ( 'NONE', ( #15448, #3685, #14832, #11314 ) ) ;
#20908 = EDGE_CURVE ( 'NONE', #14335, #15165, #8255, .T. ) ;
#20909 = EDGE_CURVE ( 'NONE', #4111, #13641, #22066, .T. ) ;
#20910 = VECTOR ( 'NONE', #16202, 1000.000000000000000 ) ;
#20911 = CYLINDRICAL_SURFACE ( 'NONE', #1460, 2.000000000000001776 ) ;
#20912 = DIRECTION ( 'NONE',  ( 0.000000000000000000, -0.000000000000000000, -1.000000000000000000 ) ) ;
#20913 = VERTEX_POINT ( 'NONE', #17409 ) ;
#20914 = AXIS2_PLACEMENT_3D ( 'NONE', #654, #13115, #12765 ) ;
#20915 = ORIENTED_EDGE ( 'NONE', *, *, #2601, .T. ) ;
#20916 = ORIENTED_EDGE ( 'NONE', *, *, #2302, .F. ) ;
#20917 = EDGE_CURVE ( 'NONE', #22529, #20860, #7406, .T. ) ;
#20918 = EDGE_LOOP ( 'NONE', ( #17935, #14101, #1154, #3088 ) ) ;
#20919 = DIRECTION ( 'NONE',  ( 0.8660254037844363761, -0.5000000000000037748, 1.141293895983254713E-15 ) ) ;
#20920 = PLANE ( 'NONE',  #4658 ) ;
#20921 = VERTEX_POINT ( 'NONE', #4940 ) ;
#20922 = EDGE_CURVE ( 'NONE', #23066, #19389, #19054, .T. ) ;
#20923 = LINE ( 'NONE', #15144, #13989 ) ;
#20924 = CARTESIAN_POINT ( 'NONE',  ( 0.3126073911696447549, 4.041451884327362798, -2.081668171172168513E-14 ) ) ;
#20925 = EDGE_CURVE ( 'NONE', #20884, #20161, #18301, .T. ) ;
#20926 = LINE ( 'NONE', #15377, #1224 ) ;
#20927 = CIRCLE ( 'NONE', #20552, 7.000000000000075495 ) ;
#20928 = DIRECTION ( 'NONE',  ( 1.399221158233658267E-15, 1.000000000000000000, -2.778352770573934118E-17 ) ) ;
#20929 = CARTESIAN_POINT ( 'NONE',  ( 3.974175853609996700, 2.726149789692757341, 2.409821656223200215 ) ) ;
#20930 = CARTESIAN_POINT ( 'NONE',  ( -8.954763739086819996, 1.387778780781445833E-14, 6.678571428571393298 ) ) ;
#20931 = AXIS2_PLACEMENT_3D ( 'NONE', #10686, #5404, #3289 ) ;
#20932 = DIRECTION ( 'NONE',  ( 1.000000000000000000, 1.479114197289397135E-31, 5.916456789157588541E-31 ) ) ;
#20933 = CARTESIAN_POINT ( 'NONE',  ( 30.00000000029184832, -0.5000000009961480529, -3.449999999999999289 ) ) ;
#20934 = CARTESIAN_POINT ( 'NONE',  ( 12.84999999999997300, -2.000000000000001776, 6.250000000000005329 ) ) ;
#20935 = DIRECTION ( 'NONE',  ( 1.000000000000000000, 0.000000000000000000, 0.000000000000000000 ) ) ;
#20936 = DIRECTION ( 'NONE',  ( 1.000000000000000000, 3.254448077276381206E-32, -1.066786462891689527E-26 ) ) ;
#20937 = CARTESIAN_POINT ( 'NONE',  ( -2.000000000000036415, 3.464101615137757495, 0.000000000000000000 ) ) ;
#20938 = EDGE_LOOP ( 'NONE', ( #12978, #5307 ) ) ;
#20939 = ORIENTED_EDGE ( 'NONE', *, *, #2060, .F. ) ;
#20940 = AXIS2_PLACEMENT_3D ( 'NONE', #6410, #1122, #11808 ) ;
#20941 = CIRCLE ( 'NONE', #21318, 0.5000000000000004441 ) ;
#20943 = ORIENTED_EDGE ( 'NONE', *, *, #2887, .T. ) ;
#20942 = ORIENTED_EDGE ( 'NONE', *, *, #13844, .T. ) ;
#20944 = CARTESIAN_POINT ( 'NONE',  ( -89.70000000000057128, -9.020562075079396891E-14, -2.000000000000001776 ) ) ;
#20945 = EDGE_CURVE ( 'NONE', #7096, #10484, #1032, .T. ) ;
#20946 = DIRECTION ( 'NONE',  ( -1.000000000000000000, -2.220446049250301001E-16, 0.000000000000000000 ) ) ;
#20947 = CARTESIAN_POINT ( 'NONE',  ( -4.751720029897110287, 36.43339712399804853, -26.00000000000000711 ) ) ;
#20948 = AXIS2_PLACEMENT_3D ( 'NONE', #19266, #1061, #3169 ) ;
#20949 = ORIENTED_EDGE ( 'NONE', *, *, #20173, .F. ) ;
#20950 = DIRECTION ( 'NONE',  ( 1.000000000000000000, 0.000000000000000000, 0.000000000000000000 ) ) ;
#20951 = DIRECTION ( 'NONE',  ( 1.000000000000000000, 0.000000000000000000, 0.000000000000000000 ) ) ;
#20952 = DIRECTION ( 'NONE',  ( 0.000000000000000000, -7.888609052210128564E-31, 1.000000000000000000 ) ) ;
#20953 = PRODUCT_DEFINITION_SHAPE ( 'NONE', 'NONE',  #7617 ) ;
#20954 = AXIS2_PLACEMENT_3D ( 'NONE', #4625, #1229, #16020 ) ;
#20955 = DIRECTION ( 'NONE',  ( 1.000000000000000000, 2.699383410053119644E-30, 3.330669073875432643E-16 ) ) ;
#20956 = CARTESIAN_POINT ( 'NONE',  ( 1.387778780781445676E-14, 4.618802153517020059, -0.3572655899081733644 ) ) ;
#20957 = DIRECTION ( 'NONE',  ( -1.000000000000000000, 4.440892098500650814E-16, 7.860214984771113767E-18 ) ) ;
#20958 = DIRECTION ( 'NONE',  ( -1.333893503340774882E-15, -2.778352770573747380E-17, -1.000000000000000000 ) ) ;
#20959 = LINE ( 'NONE', #22841, #2899 ) ;
#20960 = AXIS2_PLACEMENT_3D ( 'NONE', #7964, #18553, #12915 ) ;
#20961 = LINE ( 'NONE', #11999, #23247 ) ;
#20962 = CARTESIAN_POINT ( 'NONE',  ( 0.000000000000000000, 0.000000000000000000, 0.000000000000000000 ) ) ;
#20963 = CIRCLE ( 'NONE', #678, 6.500000000000075495 ) ;
#20964 = ORIENTED_EDGE ( 'NONE', *, *, #19177, .F. ) ;
#20965 = AXIS2_PLACEMENT_3D ( 'NONE', #22633, #13700, #20877 ) ;
#20967 = EDGE_LOOP ( 'NONE', ( #14503, #8292, #16496, #11540 ) ) ;
#20966 = ORIENTED_EDGE ( 'NONE', *, *, #16750, .F. ) ;
#20968 = VERTEX_POINT ( 'NONE', #2959 ) ;
#20970 = ORIENTED_EDGE ( 'NONE', *, *, #5079, .F. ) ;
#20969 = EDGE_LOOP ( 'NONE', ( #11880, #6945, #12355, #2751, #20216 ) ) ;
#20971 = ORIENTED_EDGE ( 'NONE', *, *, #11651, .F. ) ;
#20972 = ORIENTED_EDGE ( 'NONE', *, *, #12659, .F. ) ;
#20973 = CYLINDRICAL_SURFACE ( 'NONE', #13278, 7.000000000000075495 ) ;
#20974 = CIRCLE ( 'NONE', #1423, 4.749999999999986677 ) ;
#20975 = FACE_OUTER_BOUND ( 'NONE', #20445, .T. ) ;
#20976 = DIRECTION ( 'NONE',  ( -2.289258728441392898E-17, -0.5454545454545509653, -0.8381404052084406864 ) ) ;
#20977 = CARTESIAN_POINT ( 'NONE',  ( -12.84999999999999964, -0.5000000000000038858, 5.750000000000018652 ) ) ;
#20978 = DIRECTION ( 'NONE',  ( -1.000000000000000000, 1.389842848855773367E-62, -2.013525853228507892E-32 ) ) ;
#20979 = CARTESIAN_POINT ( 'NONE',  ( -8.165409815605727317, -2.008174044758924026, 6.581206704444227285 ) ) ;
#20980 = CIRCLE ( 'NONE', #14953, 0.5000000000000004441 ) ;
#20981 = DIRECTION ( 'NONE',  ( 4.190823558986626092E-31, -1.000000000000000000, -4.190823558986610327E-31 ) ) ;
#20982 = CARTESIAN_POINT ( 'NONE',  ( -6.000000000000116351, 1.999999999999960032, -7.500000000000062172 ) ) ;
#20983 = AXIS2_PLACEMENT_3D ( 'NONE', #8133, #20958, #1196 ) ;
#20984 = CONICAL_SURFACE ( 'NONE', #2551, 2.500000000000002220, 0.9599310885968830309 ) ;
#20985 = CARTESIAN_POINT ( 'NONE',  ( 4.158921784487734641, 2.089935040870096294, 3.499999999999967581 ) ) ;
#20986 = CARTESIAN_POINT ( 'NONE',  ( -65.00000000000046896, -0.5000000000000628386, 3.000000000000030198 ) ) ;
#20987 = EDGE_CURVE ( 'NONE', #7942, #15111, #10134, .T. ) ;
#20988 = DIRECTION ( 'NONE',  ( -7.860214984770699307E-18, 1.409037165336591006E-16, 1.000000000000000000 ) ) ;
#20989 = CARTESIAN_POINT ( 'NONE',  ( -8.391189084741235149, -12.47320284813923585, 7.111621047081351676 ) ) ;
#20990 = DIRECTION ( 'NONE',  ( 0.000000000000000000, 6.802837160693368935E-15, 1.000000000000000000 ) ) ;
#20991 = B_SPLINE_CURVE_WITH_KNOTS ( 'NONE', 3,
 ( #20607, #13427, #4475, #19180, #3070, #2837 ),
 .UNSPECIFIED., .F., .F.,
 ( 4, 2, 4 ),
 ( 0.000000000000000000, 0.0002095117440854745035, 0.0004190234881709490071 ),
 .UNSPECIFIED. ) ;
#20992 = CYLINDRICAL_SURFACE ( 'NONE', #21686, 0.4999999999999995559 ) ;
#20993 =( GEOMETRIC_REPRESENTATION_CONTEXT ( 3 ) GLOBAL_UNCERTAINTY_ASSIGNED_CONTEXT ( ( #20383 ) ) GLOBAL_UNIT_ASSIGNED_CONTEXT ( ( #17649, #22724, #23087 ) ) REPRESENTATION_CONTEXT ( 'NONE', 'WORKASPACE' ) );
#20994 = ORIENTED_EDGE ( 'NONE', *, *, #22441, .T. ) ;
#20995 = SURFACE_STYLE_USAGE ( .BOTH. , #20653 ) ;
#20997 = EDGE_LOOP ( 'NONE', ( #18156, #827 ) ) ;
#20996 = VERTEX_POINT ( 'NONE', #8363 ) ;
#20998 = ORIENTED_EDGE ( 'NONE', *, *, #6090, .T. ) ;
#20999 = CIRCLE ( 'NONE', #10844, 2.550000000000002043 ) ;
#21000 = ORIENTED_EDGE ( 'NONE', *, *, #15119, .T. ) ;
#21001 = AXIS2_PLACEMENT_3D ( 'NONE', #21711, #14871, #11326 ) ;
#21002 = EDGE_LOOP ( 'NONE', ( #8116, #6668, #16984, #8296 ) ) ;
#21003 = DIRECTION ( 'NONE',  ( 1.000000000000000000, 0.000000000000000000, 0.000000000000000000 ) ) ;
#21004 = CYLINDRICAL_SURFACE ( 'NONE', #18147, 5.999999999999991118 ) ;
#21005 = ORIENTED_EDGE ( 'NONE', *, *, #11510, .T. ) ;
#21006 = DIRECTION ( 'NONE',  ( -1.550910762415566494E-16, -1.000000000000000000, 8.135128085091684243E-31 ) ) ;
#21007 = CARTESIAN_POINT ( 'NONE',  ( 5.551115123125782702E-14, 5.499999999999980460, 2.500000000000071498 ) ) ;
#21008 = EDGE_CURVE ( 'NONE', #19367, #8320, #20959, .T. ) ;
#21009 = FACE_OUTER_BOUND ( 'NONE', #15419, .T. ) ;
#21010 = CYLINDRICAL_SURFACE ( 'NONE', #9327, 7.200000000000022382 ) ;
#21011 = DIRECTION ( 'NONE',  ( -1.000000000000000000, -2.699383410053119644E-30, -3.330669073875432643E-16 ) ) ;
#21012 = CARTESIAN_POINT ( 'NONE',  ( 4.175572532730925879, 4.122058607836116551, 1.209590929910755405E-15 ) ) ;
#21013 = EDGE_CURVE ( 'NONE', #2139, #8929, #22820, .T. ) ;
#21014 = MANIFOLD_SOLID_BREP ( 'Fillet2', #13698 ) ;
#21015 = DIRECTION ( 'NONE',  ( -0.7313537016191733464, 0.6819983600624954789, -3.733258675956564523E-18 ) ) ;
#21016 = AXIS2_PLACEMENT_3D ( 'NONE', #10657, #17841, #1717 ) ;
#21017 = CARTESIAN_POINT ( 'NONE',  ( -4.113620667976089607, 1.749999999999998002, -2.375000000000029754 ) ) ;
#21018 = DIRECTION ( 'NONE',  ( 0.9878135252003127365, -1.532010627492774434E-16, -0.1556420233463029767 ) ) ;
#21019 = CARTESIAN_POINT ( 'NONE',  ( -56.91911807125104872, -1.040834085586084257E-13, -8.333333333333413862 ) ) ;
#21020 = VERTEX_POINT ( 'NONE', #5303 ) ;
#21021 = EDGE_CURVE ( 'NONE', #17223, #555, #15532, .T. ) ;
#21022 =( NAMED_UNIT ( * ) SI_UNIT ( $, .STERADIAN. ) SOLID_ANGLE_UNIT ( ) );
#21023 = CARTESIAN_POINT ( 'NONE',  ( 3.950241966887844569, 2.668221755853158239, 2.378504353001321903 ) ) ;
#21024 = DIRECTION ( 'NONE',  ( -1.000000000000000000, 0.000000000000000000, 0.000000000000000000 ) ) ;
#21026 = EDGE_CURVE ( 'NONE', #3456, #4029, #3756, .T. ) ;
#21025 = AXIS2_PLACEMENT_3D ( 'NONE', #7405, #21762, #16441 ) ;
#21028 = ORIENTED_EDGE ( 'NONE', *, *, #3704, .T. ) ;
#21027 = VERTEX_POINT ( 'NONE', #132 ) ;
#21029 = EDGE_CURVE ( 'NONE', #6272, #9718, #4216, .T. ) ;
#21030 = ORIENTED_EDGE ( 'NONE', *, *, #15692, .F. ) ;
#21031 = ORIENTED_EDGE ( 'NONE', *, *, #1184, .F. ) ;
#21032 = EDGE_LOOP ( 'NONE', ( #9913, #16166 ) ) ;
#21033 = DIRECTION ( 'NONE',  ( -1.000000000000000000, 1.389842848855773151E-62, -2.013525853228507618E-32 ) ) ;
#21034 = CYLINDRICAL_SURFACE ( 'NONE', #3159, 2.550000000000012701 ) ;
#21035 = ORIENTED_EDGE ( 'NONE', *, *, #9823, .T. ) ;
#21036 = CARTESIAN_POINT ( 'NONE',  ( 2.681483223904249424, -3.070647092368467668, -2.185966214620738111E-14 ) ) ;
#21037 = CARTESIAN_POINT ( 'NONE',  ( -55.25320565519145788, -0.5000000000000281997, 10.00000000000009237 ) ) ;
#21038 = ADVANCED_FACE ( 'NONE', ( #21436 ), #21312, .F. ) ;
#21039 = CARTESIAN_POINT ( 'NONE',  ( 3.951447005078449148, -2.357513599190971032, 2.916666666666663410 ) ) ;
#21040 = EDGE_CURVE ( 'NONE', #9098, #21240, #17937, .T. ) ;
#21041 = CARTESIAN_POINT ( 'NONE',  ( -6.525563119752677999, 36.00216957434000165, -18.62502167978186307 ) ) ;
#21042 = DIRECTION ( 'NONE',  ( 0.000000000000000000, -3.382522293539642681E-32, -1.000000000000000000 ) ) ;
#21043 = CARTESIAN_POINT ( 'NONE',  ( -7.796097383573730610, -0.6999727310043959427, 7.943830786858171678 ) ) ;
#21044 = PRODUCT_DEFINITION_FORMATION_WITH_SPECIFIED_SOURCE ( 'ANY', '', #13999, .NOT_KNOWN. ) ;
#21045 = CARTESIAN_POINT ( 'NONE',  ( -89.70000000000059970, 2.700000000000056577, 1.000000000000000888 ) ) ;
#21046 = CYLINDRICAL_SURFACE ( 'NONE', #8191, 0.5000000000000022204 ) ;
#21047 = DIRECTION ( 'NONE',  ( 0.000000000000000000, 0.000000000000000000, 1.000000000000000000 ) ) ;
#21048 = DIRECTION ( 'NONE',  ( -1.550910762415566494E-16, -1.000000000000000000, 8.135128085091684243E-31 ) ) ;
#21049 = EDGE_CURVE ( 'NONE', #1571, #15429, #10405, .T. ) ;
#21050 = DIRECTION ( 'NONE',  ( -7.543342432310246422E-27, -0.7071067811865516806, -0.7071067811865434649 ) ) ;
#21051 = EDGE_CURVE ( 'NONE', #6614, #20569, #15279, .T. ) ;
#21052 = CYLINDRICAL_SURFACE ( 'NONE', #15324, 0.5000000000000029976 ) ;
#21053 = ORIENTED_EDGE ( 'NONE', *, *, #19181, .F. ) ;
#21054 = EDGE_CURVE ( 'NONE', #20043, #13206, #20941, .T. ) ;
#21055 = MANIFOLD_SOLID_BREP ( 'EndChamfer', #17443 ) ;
#21056 = CIRCLE ( 'NONE', #10893, 2.500000000000003997 ) ;
#21057 = ORIENTED_EDGE ( 'NONE', *, *, #14869, .T. ) ;
#21058 = CARTESIAN_POINT ( 'NONE',  ( -4.550510256924974684, 35.99999999900384751, -25.50000000000000000 ) ) ;
#21060 = EDGE_LOOP ( 'NONE', ( #7120, #10745, #5237, #6562 ) ) ;
#21059 = VERTEX_POINT ( 'NONE', #8713 ) ;
#21061 = CARTESIAN_POINT ( 'NONE',  ( -61.45000000000046469, -7.672331518739548870E-14, -2.000000000000002220 ) ) ;
#21062 = ORIENTED_EDGE ( 'NONE', *, *, #3195, .F. ) ;
#21063 = CARTESIAN_POINT ( 'NONE',  ( -3.200000000000036149, -7.500000000000027534, -7.500000000000007105 ) ) ;
#21064 = DIRECTION ( 'NONE',  ( 0.000000000000000000, 0.000000000000000000, 1.000000000000000000 ) ) ;
#21065 = EDGE_CURVE ( 'NONE', #8464, #13467, #3314, .T. ) ;
#21066 = EDGE_LOOP ( 'NONE', ( #17839, #2497, #3663, #13901 ) ) ;
#21067 = FACE_OUTER_BOUND ( 'NONE', #20771, .T. ) ;
#21068 = CARTESIAN_POINT ( 'NONE',  ( 3.951447005078456254, -1.347150628109151427, -3.500000000000006661 ) ) ;
#21069 = CARTESIAN_POINT ( 'NONE',  ( -6.999999999708142795, 13.99999999900385106, -22.50000000000000000 ) ) ;
#21070 = DIRECTION ( 'NONE',  ( -2.013525853228518840E-32, 6.902532920683810383E-31, -1.000000000000000000 ) ) ;
#21071 = DIRECTION ( 'NONE',  ( 1.000000000000000000, 2.168404344970994323E-16, -1.780660105995169760E-30 ) ) ;
#21072 = VECTOR ( 'NONE', #6830, 1000.000000000000000 ) ;
#21073 = DIRECTION ( 'NONE',  ( 7.860214984770699307E-18, -1.409037165336591006E-16, -1.000000000000000000 ) ) ;
#21074 = DIRECTION ( 'NONE',  ( -1.000000000000000000, 7.100545512326564696E-57, 1.066786462891689527E-26 ) ) ;
#21075 = EDGE_CURVE ( 'NONE', #17275, #16918, #12645, .T. ) ;
#21076 = FILL_AREA_STYLE_COLOUR ( '', #9284 ) ;
#21077 = CARTESIAN_POINT ( 'NONE',  ( -4.000000000000100364, 2.309401076758546445, -3.433295621305381573 ) ) ;
#21078 = EDGE_CURVE ( 'NONE', #138, #20968, #19995, .T. ) ;
#21079 = ORIENTED_EDGE ( 'NONE', *, *, #8765, .F. ) ;
#21080 = CARTESIAN_POINT ( 'NONE',  ( -92.38743622395925570, 28.87133558231440844, 47.16570243528394002 ) ) ;
#21082 = ORIENTED_EDGE ( 'NONE', *, *, #4082, .F. ) ;
#21081 = ORIENTED_EDGE ( 'NONE', *, *, #2920, .F. ) ;
#21083 = EDGE_LOOP ( 'NONE', ( #748, #14765, #2944, #17925 ) ) ;
#21085 = ORIENTED_EDGE ( 'NONE', *, *, #11782, .F. ) ;
#21084 = ORIENTED_EDGE ( 'NONE', *, *, #10734, .F. ) ;
#21086 = AXIS2_PLACEMENT_3D ( 'NONE', #14214, #12432, #17857 ) ;
#21087 = CIRCLE ( 'NONE', #803, 4.499999999999988454 ) ;
#21088 = CARTESIAN_POINT ( 'NONE',  ( 42.00000000000012079, 2.999999999999999112, -12.49999999999999645 ) ) ;
#21089 = FACE_OUTER_BOUND ( 'NONE', #8726, .T. ) ;
#21090 = MANIFOLD_SOLID_BREP ( 'Fillet3', #6565 ) ;
#21091 = CARTESIAN_POINT ( 'NONE',  ( 86.00000000000122213, -10.52760560296347947, -5.999999999999998224 ) ) ;
#21092 = DIRECTION ( 'NONE',  ( -0.7071067811865457964, -0.7071067811865492381, 0.000000000000000000 ) ) ;
#21093 = CARTESIAN_POINT ( 'NONE',  ( 29.00000000029184832, 16.99999999900385461, -19.49999999999998934 ) ) ;
#21094 = CARTESIAN_POINT ( 'NONE',  ( 77.42435809754135789, -4.499999999999809930, 6.500000000000137668 ) ) ;
#21095 = CARTESIAN_POINT ( 'NONE',  ( 6.000000000291855429, 2.999999999003851503, -36.44999999999999574 ) ) ;
#21096 = EDGE_CURVE ( 'NONE', #21020, #13739, #2807, .T. ) ;
#21097 = CARTESIAN_POINT ( 'NONE',  ( 42.00000000000017764, 8.000000000000003553, 2.000000000000057288 ) ) ;
#21098 = CARTESIAN_POINT ( 'NONE',  ( 0.6554360035617851077, -4.240386000424089197, -0.1586754815285195408 ) ) ;
#21099 = DIRECTION ( 'NONE',  ( -1.000000000000000000, -3.254448077276381206E-32, -1.066788928082016908E-26 ) ) ;
#21100 = CARTESIAN_POINT ( 'NONE',  ( 4.330127018922088844, -1.387778780781445676E-13, 7.500000000000027534 ) ) ;
#21101 = EDGE_CURVE ( 'NONE', #4567, #14963, #7532, .T. ) ;
#21102 = CYLINDRICAL_SURFACE ( 'NONE', #8905, 2.000000000000015543 ) ;
#21103 = CARTESIAN_POINT ( 'NONE',  ( -7.518994333257403184, -11.74196038388118879, 8.837702940568457066 ) ) ;
#21104 = CIRCLE ( 'NONE', #3792, 10.34816708862279633 ) ;
#21105 = AXIS2_PLACEMENT_3D ( 'NONE', #228, #18339, #3330 ) ;
#21106 = DIRECTION ( 'NONE',  ( -1.000000000000000000, 0.000000000000000000, -4.336808689941968432E-16 ) ) ;
#21107 = FACE_OUTER_BOUND ( 'NONE', #1574, .T. ) ;
#21108 = EDGE_CURVE ( 'NONE', #396, #14530, #12941, .T. ) ;
#21109 = VERTEX_POINT ( 'NONE', #16790 ) ;
#21110 =( BOUNDED_SURFACE ( )  B_SPLINE_SURFACE ( 3, 2, ( 
 ( #22228, #11050, #16340 ),
 ( #16788, #6114, #13288 ),
 ( #20472, #11505, #13053 ),
 ( #18687, #11279, #243 ),
 ( #2107, #12815, #5769 ),
 ( #19993, #16451, #360 ) ),
 .UNSPECIFIED., .F., .F., .T. ) 
 B_SPLINE_SURFACE_WITH_KNOTS ( ( 4, 2, 4 ),
 ( 3, 3 ),
 ( 0.01651999345535504898, 0.01858032176739834312, 0.02064065007944164074 ),
 ( 0.000000000000000000, 1.000000000000000000 ),
 .UNSPECIFIED. ) 
 GEOMETRIC_REPRESENTATION_ITEM ( )  RATIONAL_B_SPLINE_SURFACE ( (
 ( 1.000000000000000000, 0.8047781103519392465, 1.000000000000000000),
 ( 1.000000000000000000, 0.8123785825605738253, 1.000000000000000000),
 ( 1.000000000000000000, 0.8190671539786428257, 1.000000000000000000),
 ( 1.000000000000000000, 0.8192352254836726688, 1.000000000000000000),
 ( 1.000000000000000000, 0.8126129677210214286, 1.000000000000000000),
 ( 1.000000000000000000, 0.8047712537969733404, 1.000000000000000000) ) ) 
 REPRESENTATION_ITEM ( '' )  SURFACE ( )  );
#21112 = ORIENTED_EDGE ( 'NONE', *, *, #6250, .F. ) ;
#21111 = EDGE_LOOP ( 'NONE', ( #22154, #12500, #23088, #1378 ) ) ;
#21113 = ORIENTED_EDGE ( 'NONE', *, *, #7728, .F. ) ;
#21114 = EDGE_LOOP ( 'NONE', ( #19420, #8341, #9914, #14678 ) ) ;
#21115 = B_SPLINE_CURVE_WITH_KNOTS ( 'NONE', 3,
 ( #20600, #11407, #2471, #9650, #22240, #4466 ),
 .UNSPECIFIED., .F., .F.,
 ( 4, 2, 4 ),
 ( 0.007678960779285795915, 0.009067029725553659575, 0.01045509867182152497 ),
 .UNSPECIFIED. ) ;
#21116 = VERTEX_POINT ( 'NONE', #16913 ) ;
#21117 = ADVANCED_FACE ( 'NONE', ( #16683 ), #2576, .T. ) ;
#21118 = VERTEX_POINT ( 'NONE', #11394 ) ;
#21119 = DIRECTION ( 'NONE',  ( -1.066786462891689527E-26, -6.656013887802287108E-31, -1.000000000000000000 ) ) ;
#21120 = CONICAL_SURFACE ( 'NONE', #10954, 7.500000000000001776, 1.308996938995750092 ) ;
#21121 = AXIS2_PLACEMENT_3D ( 'NONE', #11589, #20668, #15225 ) ;
#21122 = FACE_OUTER_BOUND ( 'NONE', #9625, .T. ) ;
#21123 = VERTEX_POINT ( 'NONE', #3871 ) ;
#21124 = DIRECTION ( 'NONE',  ( -1.000000000000000000, 1.517883041479696593E-16, -5.334274688628647894E-15 ) ) ;
#21125 = DIRECTION ( 'NONE',  ( -1.550910762415566494E-16, -1.000000000000000000, 8.135128085091684243E-31 ) ) ;
#21126 = CARTESIAN_POINT ( 'NONE',  ( -6.000000000000088818, -2.000000000000043521, -7.500000000000007105 ) ) ;
#21127 = CARTESIAN_POINT ( 'NONE',  ( 124.5000000000018616, -6.500000000000005329, 6.500000000000179412 ) ) ;
#21128 = CARTESIAN_POINT ( 'NONE',  ( -8.223343937052021602, -0.5454750081368713310, 7.291631794411020273 ) ) ;
#21129 = FACE_OUTER_BOUND ( 'NONE', #20809, .T. ) ;
#21130 = CARTESIAN_POINT ( 'NONE',  ( 1.856282835930036383E-15, -8.271819572847245894, 11.16066016895665669 ) ) ;
#21131 = MANIFOLD_SOLID_BREP ( 'Fillet3', #20079 ) ;
#21132 = CARTESIAN_POINT ( 'NONE',  ( 3.951447005078449148, 2.357513599190909304, -2.916666666666663410 ) ) ;
#21133 = VECTOR ( 'NONE', #17440, 1000.000000000000000 ) ;
#21134 = CARTESIAN_POINT ( 'NONE',  ( 7.499999999999992895, -5.999999999999967137, 10.74999999999998224 ) ) ;
#21135 = DIRECTION ( 'NONE',  ( 0.000000000000000000, 0.000000000000000000, 1.000000000000000000 ) ) ;
#21136 = ORIENTED_EDGE ( 'NONE', *, *, #9657, .F. ) ;
#21137 = LINE ( 'NONE', #21384, #1840 ) ;
#21138 = DIRECTION ( 'NONE',  ( 2.220446049250313081E-16, -1.000000000000000000, 7.025792437124636392E-31 ) ) ;
#21139 = AXIS2_PLACEMENT_3D ( 'NONE', #12165, #13827, #6426 ) ;
#21141 = ORIENTED_EDGE ( 'NONE', *, *, #1086, .F. ) ;
#21140 = EDGE_LOOP ( 'NONE', ( #18494, #14229, #12857 ) ) ;
#21142 = AXIS2_PLACEMENT_3D ( 'NONE', #9372, #12898, #7378 ) ;
#21143 = AXIS2_PLACEMENT_3D ( 'NONE', #11009, #18540, #3953 ) ;
#21144 = AXIS2_PLACEMENT_3D ( 'NONE', #19934, #3803, #12186 ) ;
#21145 = PRODUCT_DEFINITION ( 'UNKNOWN', '', #19152, #22524 ) ;
#21146 = ORIENTED_EDGE ( 'NONE', *, *, #9248, .F. ) ;
#21147 = PRODUCT_DEFINITION_SHAPE ( 'NONE', 'NONE',  #23277 ) ;
#21148 = EDGE_LOOP ( 'NONE', ( #17653, #9951, #14936 ) ) ;
#21149 = ADVANCED_FACE ( 'NONE', ( #2819 ), #997, .T. ) ;
#21150 = CARTESIAN_POINT ( 'NONE',  ( 4.124214193018072905, 2.028338413290942555, 3.513185186763551293 ) ) ;
#21151 = DIRECTION ( 'NONE',  ( 2.013525853228507892E-32, 6.902532920683810383E-31, -1.000000000000000000 ) ) ;
#21152 = DIRECTION ( 'NONE',  ( -0.6819983600625074693, 0.7313537016191621332, -1.110084618464482116E-16 ) ) ;
#21153 = CARTESIAN_POINT ( 'NONE',  ( 0.9337610950194757953, -1.709055944985351960, 4.749999999999998224 ) ) ;
#21154 = FACE_OUTER_BOUND ( 'NONE', #8124, .T. ) ;
#21155 = EDGE_CURVE ( 'NONE', #5108, #22294, #4565, .T. ) ;
#21156 = DIRECTION ( 'NONE',  ( -3.330669073875457788E-16, -4.437342591868175641E-31, 1.000000000000000000 ) ) ;
#21157 = CIRCLE ( 'NONE', #10995, 0.5000000000000029976 ) ;
#21158 = DIRECTION ( 'NONE',  ( -2.220446049250313081E-16, 1.000000000000000000, -7.025792437124636392E-31 ) ) ;
#21159 = DIRECTION ( 'NONE',  ( -1.387778780781437314E-14, 0.000000000000000000, 1.000000000000000000 ) ) ;
#21160 = ADVANCED_FACE ( 'NONE', ( #8338 ), #947, .F. ) ;
#21161 = AXIS2_PLACEMENT_3D ( 'NONE', #11224, #16615, #15438 ) ;
#21162 = DIRECTION ( 'NONE',  ( 3.885780586188016830E-16, 4.437342591868156373E-31, -1.000000000000000000 ) ) ;
#21163 = DIRECTION ( 'NONE',  ( 0.000000000000000000, 1.000000000000000000, 0.000000000000000000 ) ) ;
#21164 = CARTESIAN_POINT ( 'NONE',  ( 0.3126073911696447549, -4.041451884327383226, 0.000000000000000000 ) ) ;
#21165 = CARTESIAN_POINT ( 'NONE',  ( 7.499999999999976907, -2.439868446130579294, 9.052558787159759035 ) ) ;
#21166 = CARTESIAN_POINT ( 'NONE',  ( 1.500000000000001332, 0.000000000000000000, 0.000000000000000000 ) ) ;
#21167 = DIRECTION ( 'NONE',  ( 0.000000000000000000, 1.000000000000000000, 0.000000000000000000 ) ) ;
#21168 = DIRECTION ( 'NONE',  ( -1.550910762415566494E-16, -1.000000000000000000, 8.135128085091684243E-31 ) ) ;
#21169 = LINE ( 'NONE', #7903, #20186 ) ;
#21170 = EDGE_LOOP ( 'NONE', ( #22730, #8826, #1413, #8820 ) ) ;
#21171 = EDGE_CURVE ( 'NONE', #15244, #4366, #19386, .T. ) ;
#21172 = CIRCLE ( 'NONE', #11008, 3.499999999999999556 ) ;
#21173 = VERTEX_POINT ( 'NONE', #3170 ) ;
#21174 = VECTOR ( 'NONE', #20231, 1000.000000000000114 ) ;
#21175 = CIRCLE ( 'NONE', #11014, 4.000000000000000888 ) ;
#21177 = EDGE_CURVE ( 'NONE', #1883, #4862, #17886, .T. ) ;
#21176 = AXIS2_PLACEMENT_3D ( 'NONE', #11635, #6363, #22948 ) ;
#21178 = CARTESIAN_POINT ( 'NONE',  ( -4.904729001339799943, 35.99999999900385461, -25.92290237457175905 ) ) ;
#21179 = CIRCLE ( 'NONE', #893, 9.500000000000063949 ) ;
#21181 = ORIENTED_EDGE ( 'NONE', *, *, #1645, .T. ) ;
#21180 = ORIENTED_EDGE ( 'NONE', *, *, #4901, .F. ) ;
#21182 = CARTESIAN_POINT ( 'NONE',  ( 77.42435809754137210, -6.499999999999811706, -5.999999999999984901 ) ) ;
#21183 = EDGE_LOOP ( 'NONE', ( #11212, #17383, #10865, #21239 ) ) ;
#21184 = LINE ( 'NONE', #5290, #12630 ) ;
#21185 = LINE ( 'NONE', #12213, #13359 ) ;
#21186 = DIRECTION ( 'NONE',  ( -1.000000000000000000, 1.276756478318923119E-15, -1.387778780781436998E-15 ) ) ;
#21188 = ORIENTED_EDGE ( 'NONE', *, *, #18875, .T. ) ;
#21187 = EDGE_CURVE ( 'NONE', #9707, #6911, #6486, .T. ) ;
#21189 = DIRECTION ( 'NONE',  ( 0.9706398123736329486, 2.155253336630096462E-16, 0.2405376366294442458 ) ) ;
#21190 = CARTESIAN_POINT ( 'NONE',  ( 0.000000000000000000, 1.750000000000001554, 0.000000000000000000 ) ) ;
#21191 = EDGE_CURVE ( 'NONE', #9565, #6270, #9876, .T. ) ;
#21192 = DIRECTION ( 'NONE',  ( 3.330669073875457788E-16, 0.000000000000000000, -1.000000000000000000 ) ) ;
#21193 = CARTESIAN_POINT ( 'NONE',  ( 4.000000000000003553, 0.000000000000000000, 0.000000000000000000 ) ) ;
#21194 = DIRECTION ( 'NONE',  ( 1.000000000000000000, 2.168404344970991858E-16, 0.000000000000000000 ) ) ;
#21195 = CIRCLE ( 'NONE', #904, 4.000000000000023093 ) ;
#21196 = VECTOR ( 'NONE', #15154, 1000.000000000000000 ) ;
#21197 = CARTESIAN_POINT ( 'NONE',  ( -3.200000000000049916, 1.999999999999911626, 7.999999999999979572 ) ) ;
#21198 = AXIS2_PLACEMENT_3D ( 'NONE', #7635, #13045, #9629 ) ;
#21199 = CARTESIAN_POINT ( 'NONE',  ( -10.49999999999995381, -2.000000000000005329, 9.249999999999966249 ) ) ;
#21200 = AXIS2_PLACEMENT_3D ( 'NONE', #21839, #5617, #13133 ) ;
#21201 = AXIS2_PLACEMENT_3D ( 'NONE', #20815, #4681, #2915 ) ;
#21202 = FACE_BOUND ( 'NONE', #3655, .T. ) ;
#21203 = EDGE_CURVE ( 'NONE', #14933, #22149, #17148, .T. ) ;
#21204 = ORIENTED_EDGE ( 'NONE', *, *, #9157, .F. ) ;
#21205 = EDGE_CURVE ( 'NONE', #7463, #5232, #18935, .T. ) ;
#21206 = EDGE_CURVE ( 'NONE', #21952, #1880, #10364, .T. ) ;
#21207 = DIRECTION ( 'NONE',  ( 0.1450682633651026177, 0.2035098390832144610, 0.9682659471243205696 ) ) ;
#21209 = ORIENTED_EDGE ( 'NONE', *, *, #2930, .F. ) ;
#21208 = VERTEX_POINT ( 'NONE', #20584 ) ;
#21210 = ORIENTED_EDGE ( 'NONE', *, *, #8635, .T. ) ;
#21211 = VECTOR ( 'NONE', #18610, 1000.000000000000000 ) ;
#21213 = ORIENTED_EDGE ( 'NONE', *, *, #1693, .F. ) ;
#21212 = VERTEX_POINT ( 'NONE', #10332 ) ;
#21214 = CLOSED_SHELL ( 'NONE', ( #19866, #5523, #8553, #8956, #22805, #11391, #5251, #21038, #15278, #22301, #12364, #13971, #7121, #8862, #17550, #2483, #17745, #13185, #20763, #9974, #363, #5213, #16686, #22041, #7117, #17996, #21911, #7621, #1214 ) ) ;
#21215 = CIRCLE ( 'NONE', #16661, 2.550000000000003819 ) ;
#21216 = ADVANCED_FACE ( 'NONE', ( #8109 ), #7992, .F. ) ;
#21217 = DIRECTION ( 'NONE',  ( -1.000000000000000000, 0.000000000000000000, 0.000000000000000000 ) ) ;
#21218 = CIRCLE ( 'NONE', #19318, 2.550000000000002043 ) ;
#21219 = CARTESIAN_POINT ( 'NONE',  ( -56.91911807125113398, 2.700000000000056577, -8.333333333333387216 ) ) ;
#21220 = LINE ( 'NONE', #3438, #21938 ) ;
#21221 = CARTESIAN_POINT ( 'NONE',  ( -2.109645605488527628E-31, 1.750000000000001554, -2.500000000000000000 ) ) ;
#21222 = EDGE_CURVE ( 'NONE', #555, #14256, #13523, .T. ) ;
#21223 = DIRECTION ( 'NONE',  ( 1.000000000000000000, -4.440892098500650814E-16, -7.860214984771115307E-18 ) ) ;
#21224 = FACE_OUTER_BOUND ( 'NONE', #8450, .T. ) ;
#21225 = DIRECTION ( 'NONE',  ( -1.000000000000000000, 0.000000000000000000, 0.000000000000000000 ) ) ;
#21226 = DIRECTION ( 'NONE',  ( -1.000000000000000000, 0.000000000000000000, 0.000000000000000000 ) ) ;
#21227 = PLANE ( 'NONE',  #22328 ) ;
#21228 = DIRECTION ( 'NONE',  ( -1.000000000000000000, -2.220446049250301001E-16, 0.000000000000000000 ) ) ;
#21229 = CARTESIAN_POINT ( 'NONE',  ( 3.878089031707361301, 0.7015470581927649718, 3.499999999999996003 ) ) ;
#21230 = DIRECTION ( 'NONE',  ( 3.885780586188016830E-16, 4.437342591868156373E-31, -1.000000000000000000 ) ) ;
#21231 = CARTESIAN_POINT ( 'NONE',  ( 5.035458327682273527, 1.561572887838372337, 0.7783303370584975234 ) ) ;
#21232 = VECTOR ( 'NONE', #14809, 1000.000000000000000 ) ;
#21233 = CARTESIAN_POINT ( 'NONE',  ( -8.200527591913225223, -12.43937801162580925, 7.318116290495828125 ) ) ;
#21234 = DIRECTION ( 'NONE',  ( 0.000000000000000000, 0.000000000000000000, -1.000000000000000000 ) ) ;
#21235 = LINE ( 'NONE', #22872, #5906 ) ;
#21236 = VERTEX_POINT ( 'NONE', #12078 ) ;
#21237 =( LENGTH_UNIT ( ) NAMED_UNIT ( * ) SI_UNIT ( .MILLI., .METRE. ) );
#21239 = ORIENTED_EDGE ( 'NONE', *, *, #18784, .F. ) ;
#21238 = ORIENTED_EDGE ( 'NONE', *, *, #2658, .T. ) ;
#21240 = VERTEX_POINT ( 'NONE', #11975 ) ;
#21241 = ORIENTED_EDGE ( 'NONE', *, *, #20162, .F. ) ;
#21242 = ORIENTED_EDGE ( 'NONE', *, *, #17604, .F. ) ;
#21243 = ADVANCED_FACE ( 'NONE', ( #6694, #19159, #10210 ), #20703, .F. ) ;
#21244 = ORIENTED_EDGE ( 'NONE', *, *, #22967, .F. ) ;
#21245 = PLANE ( 'NONE',  #2798 ) ;
#21246 = VECTOR ( 'NONE', #13751, 1000.000000000000000 ) ;
#21247 = CARTESIAN_POINT ( 'NONE',  ( 36.00000000029184832, 5.999999999003851059, -16.00000000000000000 ) ) ;
#21248 = EDGE_LOOP ( 'NONE', ( #929, #13239, #4643, #5694 ) ) ;
#21249 = FACE_OUTER_BOUND ( 'NONE', #15042, .T. ) ;
#21250 = EDGE_CURVE ( 'NONE', #23120, #5408, #6462, .T. ) ;
#21251 = DIRECTION ( 'NONE',  ( 1.000000000000000000, 6.224605580259554159E-31, -2.887593071917436153E-31 ) ) ;
#21252 = DIRECTION ( 'NONE',  ( -3.885780586188016830E-16, -4.437342591868156373E-31, 1.000000000000000000 ) ) ;
#21253 = DIRECTION ( 'NONE',  ( -1.577021341797097314E-16, 1.000000000000000000, 0.000000000000000000 ) ) ;
#21254 = CARTESIAN_POINT ( 'NONE',  ( -7.980290731945666849, -0.6082991440336598110, 7.616182555102755991 ) ) ;
#21255 = CARTESIAN_POINT ( 'NONE',  ( 4.113620667976089607, -1.750000000000025757, 2.374999999999986677 ) ) ;
#21256 = CARTESIAN_POINT ( 'NONE',  ( 42.00000000000014921, 10.49999999999999822, -6.499999999999950262 ) ) ;
#21257 = MANIFOLD_SOLID_BREP ( 'Boss-Extrude2', #23095 ) ;
#21258 = DIRECTION ( 'NONE',  ( -1.000000000000000000, -1.479114197289397135E-31, -5.916456789157588541E-31 ) ) ;
#21259 = CARTESIAN_POINT ( 'NONE',  ( 12.84999999999997300, -0.5000000000000004441, 1.387778780781445676E-14 ) ) ;
#21260 = DIRECTION ( 'NONE',  ( -0.7071067811865505703, 0.7071067811865444641, 1.010793663541190129E-16 ) ) ;
#21261 = CARTESIAN_POINT ( 'NONE',  ( 66.26395429947835680, -6.500000000000005329, -6.500000000000081712 ) ) ;
#21262 = ORIENTED_EDGE ( 'NONE', *, *, #7216, .F. ) ;
#21263 = DIRECTION ( 'NONE',  ( -0.8571428571428572063, -2.366582715663038569E-30, 0.5150787536377126052 ) ) ;
#21264 = DIRECTION ( 'NONE',  ( -2.289258728441392898E-17, -0.5454545454545509653, -0.8381404052084407974 ) ) ;
#21266 = ORIENTED_EDGE ( 'NONE', *, *, #7259, .F. ) ;
#21265 = ORIENTED_EDGE ( 'NONE', *, *, #2753, .F. ) ;
#21267 = ORIENTED_EDGE ( 'NONE', *, *, #2040, .F. ) ;
#21268 = ORIENTED_EDGE ( 'NONE', *, *, #20614, .T. ) ;
#21269 = ORIENTED_EDGE ( 'NONE', *, *, #12121, .T. ) ;
#21270 = CARTESIAN_POINT ( 'NONE',  ( 4.071447262713884463, 2.020725942163688504, -3.499999999999999556 ) ) ;
#21271 = DIRECTION ( 'NONE',  ( 0.000000000000000000, 0.000000000000000000, -1.000000000000000000 ) ) ;
#21272 = DIRECTION ( 'NONE',  ( -2.710505431213761578E-16, 1.000000000000000000, -7.518830502887770522E-31 ) ) ;
#21273 = DIRECTION ( 'NONE',  ( -0.9706398123736329486, -2.155253336630096462E-16, -0.2405376366294442458 ) ) ;
#21274 = CARTESIAN_POINT ( 'NONE',  ( -89.70000000000064233, 0.5000000000000490719, -2.000000000000001776 ) ) ;
#21275 = FACE_OUTER_BOUND ( 'NONE', #9367, .T. ) ;
#21276 = CARTESIAN_POINT ( 'NONE',  ( -7.991520206789717307, -0.6043476454136054166, 7.599114430427804656 ) ) ;
#21277 = FACE_OUTER_BOUND ( 'NONE', #13759, .T. ) ;
#21278 = DIRECTION ( 'NONE',  ( -1.000000000000000000, 0.000000000000000000, 0.000000000000000000 ) ) ;
#21279 = CARTESIAN_POINT ( 'NONE',  ( 63.53596085922838199, -4.500000000000059508, -6.000000000000060396 ) ) ;
#21280 = AXIS2_PLACEMENT_3D ( 'NONE', #20458, #19982, #3857 ) ;
#21281 = CARTESIAN_POINT ( 'NONE',  ( 7.713464495932033316, -1.828647720521569875, 8.131426806228642334 ) ) ;
#21282 = CARTESIAN_POINT ( 'NONE',  ( -7.500000000000020428, -12.00000000000002132, 9.250000000000008882 ) ) ;
#21283 = EDGE_CURVE ( 'NONE', #2097, #22821, #18814, .T. ) ;
#21284 = DIRECTION ( 'NONE',  ( -3.885780586188016830E-16, -4.437342591868156373E-31, 1.000000000000000000 ) ) ;
#21285 = CARTESIAN_POINT ( 'NONE',  ( 4.050823680195225762, -3.779313952391382792, 0.5899027668435080640 ) ) ;
#21286 = ORIENTED_EDGE ( 'NONE', *, *, #3516, .T. ) ;
#21287 = ORIENTED_EDGE ( 'NONE', *, *, #6090, .F. ) ;
#21288 =( BOUNDED_CURVE ( )  B_SPLINE_CURVE ( 3, ( #23159, #19846, #17972, #16306 ),
 .UNSPECIFIED., .F., .F. ) 
 B_SPLINE_CURVE_WITH_KNOTS ( ( 4, 4 ),
 ( 1.570796326794896558, 2.617993877991513951 ),
 .UNSPECIFIED. ) 
 CURVE ( )  GEOMETRIC_REPRESENTATION_ITEM ( )  RATIONAL_B_SPLINE_CURVE ( ( 1.000000000000000000, 0.9106836025229557707, 0.9106836025229557707, 1.000000000000000000 ) ) 
 REPRESENTATION_ITEM ( '' )  );
#21289 = DIRECTION ( 'NONE',  ( 0.000000000000000000, -6.162975822039153854E-31, -1.000000000000000000 ) ) ;
#21291 = ORIENTED_EDGE ( 'NONE', *, *, #15718, .F. ) ;
#21290 = ORIENTED_EDGE ( 'NONE', *, *, #2313, .T. ) ;
#21292 = VECTOR ( 'NONE', #96, 1000.000000000000000 ) ;
#21293 = EDGE_CURVE ( 'NONE', #21020, #12892, #12438, .T. ) ;
#21294 = CARTESIAN_POINT ( 'NONE',  ( 0.000000000000000000, 1.750000000000001554, 0.000000000000000000 ) ) ;
#21295 = DIRECTION ( 'NONE',  ( -1.066786462891689527E-26, -6.656013887802287108E-31, -1.000000000000000000 ) ) ;
#21296 = B_SPLINE_CURVE_WITH_KNOTS ( 'NONE', 3,
 ( #3047, #6461, #22352, #2929 ),
 .UNSPECIFIED., .F., .F.,
 ( 4, 4 ),
 ( 2.380737581673407957E-07, 0.002336974151641583747 ),
 .UNSPECIFIED. ) ;
#21297 = CARTESIAN_POINT ( 'NONE',  ( 2.775557561562891351E-14, 7.999999999999983125, 2.500000000000057732 ) ) ;
#21298 = VECTOR ( 'NONE', #15474, 1000.000000000000000 ) ;
#21299 = CARTESIAN_POINT ( 'NONE',  ( 0.000000000000000000, 0.000000000000000000, 0.000000000000000000 ) ) ;
#21300 = ORIENTED_EDGE ( 'NONE', *, *, #15183, .F. ) ;
#21301 = CIRCLE ( 'NONE', #14157, 0.5000000000000019984 ) ;
#21302 = CARTESIAN_POINT ( 'NONE',  ( 6.999999999999992006, -5.999999999999981348, 12.25000000000001066 ) ) ;
#21303 = CARTESIAN_POINT ( 'NONE',  ( -12.85000000000005649, -12.00000000000011191, -6.249999999999936051 ) ) ;
#21304 = AXIS2_PLACEMENT_3D ( 'NONE', #18486, #7446, #16481 ) ;
#21305 = CARTESIAN_POINT ( 'NONE',  ( 0.1397371499203187151, 1.362866705341262197, -3.500000000000009770 ) ) ;
#21306 = CARTESIAN_POINT ( 'NONE',  ( -6.999999999708142795, 49.99999999900385461, -26.00000000000000711 ) ) ;
#21307 = ADVANCED_FACE ( 'NONE', ( #19509 ), #18876, .F. ) ;
#21308 = CYLINDRICAL_SURFACE ( 'NONE', #2432, 0.2500000000000002220 ) ;
#21309 = CARTESIAN_POINT ( 'NONE',  ( -4.000000000000098588, -1.560351142792954393, -0.2242961665060443921 ) ) ;
#21310 = DIRECTION ( 'NONE',  ( 7.860214984771176937E-18, 1.409037165336591006E-16, 1.000000000000000000 ) ) ;
#21311 = FACE_OUTER_BOUND ( 'NONE', #14080, .T. ) ;
#21312 = PLANE ( 'NONE',  #11515 ) ;
#21313 = EDGE_CURVE ( 'NONE', #18075, #6443, #17124, .T. ) ;
#21314 = AXIS2_PLACEMENT_3D ( 'NONE', #8215, #10095, #12065 ) ;
#21315 = DIRECTION ( 'NONE',  ( -1.000000000000000000, -2.220446049250301001E-16, 0.000000000000000000 ) ) ;
#21316 = ORIENTED_EDGE ( 'NONE', *, *, #5543, .F. ) ;
#21317 = AXIS2_PLACEMENT_3D ( 'NONE', #6148, #2488, #15063 ) ;
#21318 = AXIS2_PLACEMENT_3D ( 'NONE', #9060, #10708, #5541 ) ;
#21319 = ADVANCED_FACE ( 'NONE', ( #19622 ), #1737, .T. ) ;
#21320 = EDGE_CURVE ( 'NONE', #7483, #17574, #16845, .T. ) ;
#21322 = VERTEX_POINT ( 'NONE', #21638 ) ;
#21321 = ORIENTED_EDGE ( 'NONE', *, *, #14053, .T. ) ;
#21323 = CIRCLE ( 'NONE', #23156, 3.749999999999989786 ) ;
#21324 = ORIENTED_EDGE ( 'NONE', *, *, #18037, .F. ) ;
#21325 = AXIS2_PLACEMENT_3D ( 'NONE', #11569, #4275, #21747 ) ;
#21327 = ORIENTED_EDGE ( 'NONE', *, *, #22604, .T. ) ;
#21326 = ORIENTED_EDGE ( 'NONE', *, *, #14111, .F. ) ;
#21328 = CARTESIAN_POINT ( 'NONE',  ( -5.623500955413153868, 35.99999999900385461, -25.73132293306449370 ) ) ;
#21329 = CARTESIAN_POINT ( 'NONE',  ( 5.600000000000000533, -4.041451884327432076, -6.938893903907228378E-15 ) ) ;
#21330 =( NAMED_UNIT ( * ) PLANE_ANGLE_UNIT ( ) SI_UNIT ( $, .RADIAN. ) );
#21331 = CYLINDRICAL_SURFACE ( 'NONE', #18471, 2.549999999999997158 ) ;
#21332 = DIRECTION ( 'NONE',  ( 1.000000000000000000, 1.479114197289387852E-30, -2.013525853228518840E-32 ) ) ;
#21333 = AXIS2_PLACEMENT_3D ( 'NONE', #2685, #2229, #4102 ) ;
#21334 = CARTESIAN_POINT ( 'NONE',  ( 27.99999999999991118, 9.183364406542126228E-15, -2.500000000000028422 ) ) ;
#21335 = EDGE_CURVE ( 'NONE', #19516, #16622, #10006, .T. ) ;
#21336 = CARTESIAN_POINT ( 'NONE',  ( 42.00000000000020606, 2.999999999999999112, -0.4999999999999449329 ) ) ;
#21337 = CIRCLE ( 'NONE', #8175, 2.499999999999990674 ) ;
#21338 = EDGE_CURVE ( 'NONE', #18076, #4111, #6806, .T. ) ;
#21339 = EDGE_CURVE ( 'NONE', #7176, #13355, #5037, .T. ) ;
#21340 = CARTESIAN_POINT ( 'NONE',  ( 0.000000000000000000, 0.000000000000000000, -5.600000000000000533 ) ) ;
#21341 = FACE_BOUND ( 'NONE', #19459, .T. ) ;
#21342 = CARTESIAN_POINT ( 'NONE',  ( 3.861362476283208167, 2.629030857715989988, -3.671615880910374941 ) ) ;
#21343 = AXIS2_PLACEMENT_3D ( 'NONE', #20233, #16446, #11498 ) ;
#21344 = FACE_OUTER_BOUND ( 'NONE', #21002, .T. ) ;
#21345 = CARTESIAN_POINT ( 'NONE',  ( -56.54644007500103697, -2.700000000000084110, -8.666666666666710483 ) ) ;
#21346 = AXIS2_PLACEMENT_3D ( 'NONE', #2869, #15670, #13805 ) ;
#21347 = DIRECTION ( 'NONE',  ( -5.598259082250514647E-17, 1.000000000000000000, -6.162975822039315660E-32 ) ) ;
#21348 = EDGE_CURVE ( 'NONE', #3913, #1642, #5071, .T. ) ;
#21349 = DIRECTION ( 'NONE',  ( -1.000000000000000000, 2.168404344970992105E-16, 3.469446951953587368E-15 ) ) ;
#21350 = PRODUCT ( 'Lock nut', 'Lock nut', '', ( #3206 ) ) ;
#21351 = CONICAL_SURFACE ( 'NONE', #13442, 3.500000000000004441, 1.047197551196600296 ) ;
#21352 = VERTEX_POINT ( 'NONE', #440 ) ;
#21353 = EDGE_CURVE ( 'NONE', #1834, #4926, #5880, .T. ) ;
#21354 = SHAPE_REPRESENTATION_RELATIONSHIP ( 'NONE' , 'NONE' ,  #16280, #6953 ) ;
#21355 = AXIS2_PLACEMENT_3D ( 'NONE', #2815, #9992, #6457 ) ;
#21357 = EDGE_LOOP ( 'NONE', ( #1011, #3583, #14359, #19518 ) ) ;
#21356 = ORIENTED_EDGE ( 'NONE', *, *, #19456, .T. ) ;
#21358 = EDGE_CURVE ( 'NONE', #9332, #6633, #11023, .T. ) ;
#21359 = AXIS2_PLACEMENT_3D ( 'NONE', #13947, #21264, #16053 ) ;
#21360 = ORIENTED_EDGE ( 'NONE', *, *, #9642, .F. ) ;
#21362 = ORIENTED_EDGE ( 'NONE', *, *, #12803, .T. ) ;
#21361 = ORIENTED_EDGE ( 'NONE', *, *, #11390, .F. ) ;
#21363 = ORIENTED_EDGE ( 'NONE', *, *, #9941, .T. ) ;
#21364 = ORIENTED_EDGE ( 'NONE', *, *, #12267, .F. ) ;
#21365 = DIRECTION ( 'NONE',  ( 1.000000000000000000, 0.000000000000000000, 0.000000000000000000 ) ) ;
#21366 = AXIS2_PLACEMENT_3D ( 'NONE', #10237, #8137, #2842 ) ;
#21367 = CIRCLE ( 'NONE', #702, 4.607329295533694413 ) ;
#21368 = CARTESIAN_POINT ( 'NONE',  ( 0.000000000000000000, 1.750000000000001554, 0.000000000000000000 ) ) ;
#21369 = ORIENTED_EDGE ( 'NONE', *, *, #1628, .T. ) ;
#21370 = CARTESIAN_POINT ( 'NONE',  ( 63.50658097017377912, -4.000000000000003553, 6.500000000000151879 ) ) ;
#21371 = DIRECTION ( 'NONE',  ( 1.000000000000000000, 3.254448077276381206E-32, 1.066788928082016908E-26 ) ) ;
#21372 = DIRECTION ( 'NONE',  ( -1.000000000000000000, 0.000000000000000000, 0.000000000000000000 ) ) ;
#21373 = CARTESIAN_POINT ( 'NONE',  ( 81.85734743794773749, -6.246200939475199831, 6.500000000000130562 ) ) ;
#21374 = FACE_OUTER_BOUND ( 'NONE', #4748, .T. ) ;
#21375 = CARTESIAN_POINT ( 'NONE',  ( 36.00000000029184832, 16.99999999900385461, -18.50000000000000355 ) ) ;
#21376 = CARTESIAN_POINT ( 'NONE',  ( 57.49335071782236639, -0.7089083427137543580, 6.000000000000143885 ) ) ;
#21377 = CIRCLE ( 'NONE', #11208, 4.000000000000000888 ) ;
#21378 = DIRECTION ( 'NONE',  ( -4.190823558986625216E-31, 1.000000000000000000, -4.190823558986625216E-31 ) ) ;
#21379 = CARTESIAN_POINT ( 'NONE',  ( 0.000000000000000000, 2.499999999999998668, 0.000000000000000000 ) ) ;
#21380 = EDGE_CURVE ( 'NONE', #16893, #10242, #18214, .T. ) ;
#21381 = CARTESIAN_POINT ( 'NONE',  ( 29.00000000029184832, 16.99999999900385461, -29.00000000000000355 ) ) ;
#21382 = EDGE_LOOP ( 'NONE', ( #21810, #22638, #7300, #4923 ) ) ;
#21383 = AXIS2_PLACEMENT_3D ( 'NONE', #12079, #17503, #8463 ) ;
#21384 = CARTESIAN_POINT ( 'NONE',  ( -12.84999999999999964, -6.938893903907228378E-15, 5.749999999999991118 ) ) ;
#21385 = TOROIDAL_SURFACE ( 'NONE', #21325, 3.500000000000000000, 0.5000000000000000000 ) ;
#21386 = PLANE ( 'NONE',  #5925 ) ;
#21387 = TOROIDAL_SURFACE ( 'NONE', #11967, 7.882182279042408979, 2.500000000000000000 ) ;
#21389 = ORIENTED_EDGE ( 'NONE', *, *, #19000, .T. ) ;
#21388 = ORIENTED_EDGE ( 'NONE', *, *, #2806, .T. ) ;
#21390 = ADVANCED_FACE ( 'NONE', ( #7730, #20092, #680 ), #15013, .F. ) ;
#21391 = ORIENTED_EDGE ( 'NONE', *, *, #9946, .F. ) ;
#21392 = ORIENTED_EDGE ( 'NONE', *, *, #20303, .F. ) ;
#21393 = MECHANICAL_DESIGN_GEOMETRIC_PRESENTATION_REPRESENTATION (  '', ( #338 ), #9722 ) ;
#21394 = CARTESIAN_POINT ( 'NONE',  ( -3.999999999708139686, 49.99999999900386172, -29.00000000000000355 ) ) ;
#21395 = VECTOR ( 'NONE', #4822, 1000.000000000000227 ) ;
#21396 = CARTESIAN_POINT ( 'NONE',  ( 8.223343937052055352, -0.5454750081368732184, 7.291631794411076228 ) ) ;
#21397 = ADVANCED_FACE ( 'NONE', ( #2312 ), #4080, .T. ) ;
#21398 = CARTESIAN_POINT ( 'NONE',  ( 3.950241966888151435, 3.393956070637460520, -1.121495646999018270 ) ) ;
#21399 = CARTESIAN_POINT ( 'NONE',  ( 4.170895651974849905, -2.054890354522451279, -3.559174498016467680 ) ) ;
#21400 = CIRCLE ( 'NONE', #10859, 0.4999999999999999445 ) ;
#21401 =( BOUNDED_SURFACE ( )  B_SPLINE_SURFACE ( 3, 2, ( 
 ( #3755, #18011, #5430 ),
 ( #10706, #23194, #17891 ),
 ( #10923, #12587, #14476 ),
 ( #1873, #19773, #9059 ),
 ( #12223, #16101, #5067 ),
 ( #19410, #8712, #15868 ) ),
 .UNSPECIFIED., .F., .F., .T. ) 
 B_SPLINE_SURFACE_WITH_KNOTS ( ( 4, 2, 4 ),
 ( 3, 3 ),
 ( 0.01651999345535502470, 0.01858032176739832578, 0.02064065007944162686 ),
 ( 0.000000000000000000, 1.000000000000000000 ),
 .UNSPECIFIED. ) 
 GEOMETRIC_REPRESENTATION_ITEM ( )  RATIONAL_B_SPLINE_SURFACE ( (
 ( 1.000000000000000000, 0.8047781103519390244, 1.000000000000000000),
 ( 1.000000000000000000, 0.8123785825604251665, 1.000000000000000000),
 ( 1.000000000000000000, 0.8190671539788410005, 1.000000000000000000),
 ( 1.000000000000000000, 0.8192352254834731617, 1.000000000000000000),
 ( 1.000000000000000000, 0.8126129677211720859, 1.000000000000000000),
 ( 1.000000000000000000, 0.8047712537969733404, 1.000000000000000000) ) ) 
 REPRESENTATION_ITEM ( '' )  SURFACE ( )  );
#21402 = DIRECTION ( 'NONE',  ( -2.775557561562887961E-17, 2.857733511404945646E-16, -1.000000000000000000 ) ) ;
#21403 = CARTESIAN_POINT ( 'NONE',  ( -6.938893903907228378E-14, -4.618802153517121312, -3.433295621305409107 ) ) ;
#21404 = DIRECTION ( 'NONE',  ( -1.000000000000000000, 0.000000000000000000, 0.000000000000000000 ) ) ;
#21405 = DIRECTION ( 'NONE',  ( 0.000000000000000000, 0.000000000000000000, 1.000000000000000000 ) ) ;
#21406 = CARTESIAN_POINT ( 'NONE',  ( 116.5066492821802768, -7.708908342713760575, 6.500000000000151879 ) ) ;
#21407 = CARTESIAN_POINT ( 'NONE',  ( 37.43301270189239460, 10.75000000000000178, -10.00000000000007994 ) ) ;
#21408 = DIRECTION ( 'NONE',  ( 8.438582421954109416E-32, 0.000000000000000000, 1.000000000000000000 ) ) ;
#21409 = CARTESIAN_POINT ( 'NONE',  ( 1.500000000000001332, 0.000000000000000000, 0.000000000000000000 ) ) ;
#21410 = EDGE_CURVE ( 'NONE', #6978, #16151, #14901, .T. ) ;
#21411 = CARTESIAN_POINT ( 'NONE',  ( -6.938893903907228378E-15, 1.500000000000001332, 0.000000000000000000 ) ) ;
#21412 = PLANE ( 'NONE',  #13433 ) ;
#21413 = EDGE_LOOP ( 'NONE', ( #7680, #21651, #9243, #6642 ) ) ;
#21414 = EDGE_CURVE ( 'NONE', #12422, #9827, #16741, .T. ) ;
#21415 = AXIS2_PLACEMENT_3D ( 'NONE', #10498, #12726, #2015 ) ;
#21416 = EDGE_LOOP ( 'NONE', ( #16466, #1327 ) ) ;
#21417 = CARTESIAN_POINT ( 'NONE',  ( -4.993857080232831258, 35.99999999900384751, -25.53590495946178152 ) ) ;
#21419 = ORIENTED_EDGE ( 'NONE', *, *, #5841, .F. ) ;
#21418 = ORIENTED_EDGE ( 'NONE', *, *, #4458, .F. ) ;
#21420 = VECTOR ( 'NONE', #11039, 1000.000000000000000 ) ;
#21421 = CARTESIAN_POINT ( 'NONE',  ( 2.807080416179122295, -3.225969019225178425, -3.502507215260535656 ) ) ;
#21422 = DIRECTION ( 'NONE',  ( 0.000000000000000000, 0.000000000000000000, 1.000000000000000000 ) ) ;
#21423 = AXIS2_PLACEMENT_3D ( 'NONE', #21080, #12229, #22848 ) ;
#21424 = DIRECTION ( 'NONE',  ( 5.551115123125797493E-17, -2.869019762633797485E-16, -1.000000000000000000 ) ) ;
#21425 = ADVANCED_FACE ( 'NONE', ( #16423, #22085 ), #11139, .F. ) ;
#21426 = CARTESIAN_POINT ( 'NONE',  ( -2.000000000000015543, 3.464101615137746837, -5.600000000000000533 ) ) ;
#21427 = EDGE_LOOP ( 'NONE', ( #13618, #16596, #15571, #15219 ) ) ;
#21428 = DIRECTION ( 'NONE',  ( -1.000000000000000000, -3.254448077276381206E-32, -1.066788928082016908E-26 ) ) ;
#21429 = CARTESIAN_POINT ( 'NONE',  ( -50.65685424949263904, -7.200000000000071232, -7.500000000000034639 ) ) ;
#21430 = DIRECTION ( 'NONE',  ( 1.392757777031969319E-14, 1.000000000000000000, -5.941108692445745160E-30 ) ) ;
#21431 = CARTESIAN_POINT ( 'NONE',  ( -1.387778780781445676E-14, -8.271819572847247670, 0.000000000000000000 ) ) ;
#21432 = FACE_OUTER_BOUND ( 'NONE', #2352, .T. ) ;
#21433 = CARTESIAN_POINT ( 'NONE',  ( 8.719386969281730515, -1.499999991380386533, 6.820015264002347699 ) ) ;
#21434 = CARTESIAN_POINT ( 'NONE',  ( 2.775557561562891351E-14, 2.999999999999992450, -0.4999999999999865663 ) ) ;
#21435 = DIRECTION ( 'NONE',  ( -1.000000000000000000, 0.000000000000000000, 0.000000000000000000 ) ) ;
#21436 = FACE_OUTER_BOUND ( 'NONE', #17871, .T. ) ;
#21437 = DIRECTION ( 'NONE',  ( -1.000000000000000000, -6.224605580259554159E-31, 2.887593071917436153E-31 ) ) ;
#21438 = CIRCLE ( 'NONE', #8276, 3.000000000000011546 ) ;
#21439 = FACE_OUTER_BOUND ( 'NONE', #19451, .T. ) ;
#21440 = ORIENTED_EDGE ( 'NONE', *, *, #519, .T. ) ;
#21441 = APPLICATION_PROTOCOL_DEFINITION ( 'draft international standard', 'automotive_design', 1998, #8638 ) ;
#21443 = ORIENTED_EDGE ( 'NONE', *, *, #1321, .T. ) ;
#21442 = EDGE_LOOP ( 'NONE', ( #20420, #19864, #18735 ) ) ;
#21444 = EDGE_LOOP ( 'NONE', ( #13098, #13380, #17013, #6912, #1102, #4495, #13704, #20710 ) ) ;
#21446 = ORIENTED_EDGE ( 'NONE', *, *, #3077, .F. ) ;
#21445 = ORIENTED_EDGE ( 'NONE', *, *, #5513, .T. ) ;
#21447 = LINE ( 'NONE', #16229, #9885 ) ;
#21448 = CYLINDRICAL_SURFACE ( 'NONE', #5836, 2.999999999999999112 ) ;
#21449 = EDGE_CURVE ( 'NONE', #15111, #688, #2431, .T. ) ;
#21450 = CARTESIAN_POINT ( 'NONE',  ( 7.324400034341882026, -11.76702354778242920, 7.601326208249671978 ) ) ;
#21451 = CYLINDRICAL_SURFACE ( 'NONE', #8706, 4.750000000000013323 ) ;
#21452 = FACE_OUTER_BOUND ( 'NONE', #10435, .T. ) ;
#21453 = CARTESIAN_POINT ( 'NONE',  ( -8.414481090081508796, 1.743352624126960279E-14, 6.435353702847428359 ) ) ;
#21454 = CARTESIAN_POINT ( 'NONE',  ( 3.674234614174737068, -0.7499999999999451550, -3.000000000000002665 ) ) ;
#21455 =( NAMED_UNIT ( * ) PLANE_ANGLE_UNIT ( ) SI_UNIT ( $, .RADIAN. ) );
#21456 = ADVANCED_FACE ( 'NONE', ( #5978 ), #11502, .T. ) ;
#21457 = DIRECTION ( 'NONE',  ( 1.000000000000000000, 0.000000000000000000, 0.000000000000000000 ) ) ;
#21458 = CARTESIAN_POINT ( 'NONE',  ( 3.510273485745285083, 2.827716139362673076, -3.610536846335890449 ) ) ;
#21459 = CARTESIAN_POINT ( 'NONE',  ( 2.775557561562891351E-14, 11.00000000000000000, -9.999999999999968026 ) ) ;
#21460 = ADVANCED_FACE ( 'NONE', ( #20321 ), #22038, .F. ) ;
#21461 = LINE ( 'NONE', #5097, #8574 ) ;
#21462 = CARTESIAN_POINT ( 'NONE',  ( 7.268749084027611218, -2.258953384213798987, 7.689023314178105473 ) ) ;
#21463 = DIRECTION ( 'NONE',  ( 0.000000000000000000, 0.000000000000000000, 1.000000000000000000 ) ) ;
#21464 = DIRECTION ( 'NONE',  ( -3.330669073875432643E-16, -4.437342591868153746E-31, 1.000000000000000000 ) ) ;
#21465 = ORIENTED_EDGE ( 'NONE', *, *, #18844, .F. ) ;
#21466 = AXIS2_PLACEMENT_3D ( 'NONE', #3192, #15639, #22832 ) ;
#21468 = ORIENTED_EDGE ( 'NONE', *, *, #10960, .T. ) ;
#21467 = EDGE_LOOP ( 'NONE', ( #3604, #598, #22612, #1806 ) ) ;
#21469 = EDGE_LOOP ( 'NONE', ( #17453, #15449, #10145, #20456 ) ) ;
#21470 = EDGE_CURVE ( 'NONE', #7255, #16805, #625, .T. ) ;
#21471 = EDGE_CURVE ( 'NONE', #8320, #16118, #3995, .T. ) ;
#21473 = ORIENTED_EDGE ( 'NONE', *, *, #21075, .T. ) ;
#21472 = ORIENTED_EDGE ( 'NONE', *, *, #13820, .T. ) ;
#21474 = ORIENTED_EDGE ( 'NONE', *, *, #8981, .F. ) ;
#21475 = EDGE_LOOP ( 'NONE', ( #2274, #16325, #7346, #18734 ) ) ;
#21476 = EDGE_CURVE ( 'NONE', #14170, #12207, #18647, .T. ) ;
#21477 = EDGE_LOOP ( 'NONE', ( #5896, #13302, #21557, #1716 ) ) ;
#21478 = DIRECTION ( 'NONE',  ( -1.000000000000000000, -4.440892098500626162E-16, 5.551115123125782702E-16 ) ) ;
#21479 = CARTESIAN_POINT ( 'NONE',  ( -43.46238456605044576, 4.919238815542508192, -7.500000000000034639 ) ) ;
#21480 = CARTESIAN_POINT ( 'NONE',  ( -7.500000000000034639, -12.60977222864646485, 9.250000000000063949 ) ) ;
#21481 = DIRECTION ( 'NONE',  ( 1.333893503340766797E-15, -2.778352770574087576E-17, -1.000000000000000000 ) ) ;
#21482 = EDGE_CURVE ( 'NONE', #4281, #1910, #9733, .T. ) ;
#21483 = CARTESIAN_POINT ( 'NONE',  ( 12.84999999999997300, 0.000000000000000000, 1.387778780781445676E-14 ) ) ;
#21484 = DIRECTION ( 'NONE',  ( -0.000000000000000000, -0.000000000000000000, -1.000000000000000000 ) ) ;
#21485 = AXIS2_PLACEMENT_3D ( 'NONE', #13393, #2569, #9866 ) ;
#21486 = AXIS2_PLACEMENT_3D ( 'NONE', #2481, #13432, #22134 ) ;
#21487 = CARTESIAN_POINT ( 'NONE',  ( -4.101948962586009273, 2.368261337751074169, -3.681124513963648148 ) ) ;
#21488 = SURFACE_STYLE_USAGE ( .BOTH. , #21713 ) ;
#21489 = CARTESIAN_POINT ( 'NONE',  ( -65.00000000000052580, 2.700000000000063238, 3.000000000000002665 ) ) ;
#21490 = DIRECTION ( 'NONE',  ( 1.000000000000000000, 1.479114197289388027E-30, -2.013525853228518840E-32 ) ) ;
#21491 = LINE ( 'NONE', #21134, #17811 ) ;
#21492 = CARTESIAN_POINT ( 'NONE',  ( -8.954763739086851970, -1.500000000000001332, 6.678571428571422608 ) ) ;
#21493 = ORIENTED_EDGE ( 'NONE', *, *, #5708, .F. ) ;
#21494 =( NAMED_UNIT ( * ) SI_UNIT ( $, .STERADIAN. ) SOLID_ANGLE_UNIT ( ) );
#21495 = DIRECTION ( 'NONE',  ( 1.733449886265891589E-32, -4.190823558986610327E-31, 1.000000000000000000 ) ) ;
#21496 = DIRECTION ( 'NONE',  ( -0.8122328620674111876, 0.000000000000000000, -0.5833333333333368120 ) ) ;
#21498 = VERTEX_POINT ( 'NONE', #11478 ) ;
#21497 = ORIENTED_EDGE ( 'NONE', *, *, #20527, .T. ) ;
#21499 = EDGE_CURVE ( 'NONE', #3480, #10125, #8437, .T. ) ;
#21500 = EDGE_CURVE ( 'NONE', #16775, #5606, #20799, .T. ) ;
#21501 = VERTEX_POINT ( 'NONE', #18785 ) ;
#21502 = VECTOR ( 'NONE', #6769, 1000.000000000000114 ) ;
#21503 = AXIS2_PLACEMENT_3D ( 'NONE', #3216, #14262, #17543 ) ;
#21504 = ORIENTED_EDGE ( 'NONE', *, *, #5936, .T. ) ;
#21505 = EDGE_LOOP ( 'NONE', ( #8524, #17122, #9564, #17418, #7830, #12622, #16253, #7600 ) ) ;
#21506 = LINE ( 'NONE', #23031, #23084 ) ;
#21507 = DIRECTION ( 'NONE',  ( -1.000000000000000000, -1.910522504832140594E-31, 5.551115123125818447E-17 ) ) ;
#21508 = EDGE_CURVE ( 'NONE', #7853, #8658, #7958, .T. ) ;
#21509 = DIRECTION ( 'NONE',  ( 1.000000000000000000, 0.000000000000000000, -1.613696256722611405E-16 ) ) ;
#21510 = DIRECTION ( 'NONE',  ( -1.107262168541282614E-16, 1.107262168541365321E-16, -1.000000000000000000 ) ) ;
#21511 = CIRCLE ( 'NONE', #19627, 2.550000000000003819 ) ;
#21512 = DIRECTION ( 'NONE',  ( -4.336808689941983223E-16, 0.000000000000000000, 1.000000000000000000 ) ) ;
#21513 = DIRECTION ( 'NONE',  ( 1.000000000000000000, 0.000000000000000000, 0.000000000000000000 ) ) ;
#21514 = CARTESIAN_POINT ( 'NONE',  ( 24.74999999999994316, 6.938893903907228378E-14, -17.00000000000001066 ) ) ;
#21515 = FACE_OUTER_BOUND ( 'NONE', #15213, .T. ) ;
#21516 = DIRECTION ( 'NONE',  ( -3.330669073875432643E-16, -4.437342591868153746E-31, 1.000000000000000000 ) ) ;
#21517 = DIRECTION ( 'NONE',  ( 2.013525853228507892E-32, 6.902532920683810383E-31, -1.000000000000000000 ) ) ;
#21518 = AXIS2_PLACEMENT_3D ( 'NONE', #22100, #6338, #7864 ) ;
#21519 = DIRECTION ( 'NONE',  ( -1.550910762415566494E-16, -1.000000000000000000, 8.135128085091684243E-31 ) ) ;
#21520 = CYLINDRICAL_SURFACE ( 'NONE', #1776, 0.2500000000000002220 ) ;
#21521 = CARTESIAN_POINT ( 'NONE',  ( -1.360585162436302342, 4.061296242127595768, -3.505054077164885928 ) ) ;
#21522 = CIRCLE ( 'NONE', #11342, 2.499999999999993339 ) ;
#21523 = FACE_OUTER_BOUND ( 'NONE', #1603, .T. ) ;
#21524 = CARTESIAN_POINT ( 'NONE',  ( 3.972709601346605890, -2.746729940827227434, 2.374099244652743135 ) ) ;
#21525 = ORIENTED_EDGE ( 'NONE', *, *, #14288, .T. ) ;
#21526 = ORIENTED_EDGE ( 'NONE', *, *, #5991, .T. ) ;
#21527 = FACE_OUTER_BOUND ( 'NONE', #5234, .T. ) ;
#21528 = ORIENTED_EDGE ( 'NONE', *, *, #16419, .F. ) ;
#21529 = CIRCLE ( 'NONE', #22645, 0.5000000000000038858 ) ;
#21530 = CONICAL_SURFACE ( 'NONE', #6488, 4.000000000000000000, 1.047197551196595855 ) ;
#21531 = PLANE ( 'NONE',  #9166 ) ;
#21532 = AXIS2_PLACEMENT_3D ( 'NONE', #3719, #10888, #18082 ) ;
#21533 = CIRCLE ( 'NONE', #479, 2.549999999999997158 ) ;
#21534 = FACE_OUTER_BOUND ( 'NONE', #12598, .T. ) ;
#21535 = CARTESIAN_POINT ( 'NONE',  ( 7.268749084027636975, -11.74104661578624409, 7.689023314178095703 ) ) ;
#21536 = TOROIDAL_SURFACE ( 'NONE', #14381, 4.500000000000002665, 0.5000000000000000000 ) ;
#21537 = CARTESIAN_POINT ( 'NONE',  ( 124.5000000000019043, -6.500000000000005329, 6.000000000000165201 ) ) ;
#21538 = ORIENTED_EDGE ( 'NONE', *, *, #8798, .F. ) ;
#21539 = CARTESIAN_POINT ( 'NONE',  ( 5.051814855409154426, 4.882486540518890195, -6.250000000000007105 ) ) ;
#21540 = CARTESIAN_POINT ( 'NONE',  ( 0.03027795056223035047, 0.6888063905604809856, 3.499999999999959144 ) ) ;
#21541 = FACE_OUTER_BOUND ( 'NONE', #14907, .T. ) ;
#21542 = EDGE_CURVE ( 'NONE', #19955, #18025, #15361, .T. ) ;
#21543 = CARTESIAN_POINT ( 'NONE',  ( 1.655952806101401054, -3.662737355149109142, -4.567116948300461998E-14 ) ) ;
#21544 = CARTESIAN_POINT ( 'NONE',  ( 88.75737332930593482, -6.527605602963476805, -6.499999999999929834 ) ) ;
#21545 = DIRECTION ( 'NONE',  ( 2.172745813409349776E-17, -1.000000000000000000, 1.309377075419428048E-16 ) ) ;
#21546 = CARTESIAN_POINT ( 'NONE',  ( 4.151274195509685683, 2.039912954708771320, -3.533232880573506485 ) ) ;
#21547 = DIRECTION ( 'NONE',  ( 4.190823558986625216E-31, -1.000000000000000000, 4.190823558986625216E-31 ) ) ;
#21548 = AXIS2_PLACEMENT_3D ( 'NONE', #2839, #9899, #17405 ) ;
#21549 = CARTESIAN_POINT ( 'NONE',  ( 119.5756419024615553, -11.00000000000006573, 6.500000000000012434 ) ) ;
#21550 = AXIS2_PLACEMENT_3D ( 'NONE', #22836, #6715, #10129 ) ;
#21551 = AXIS2_PLACEMENT_3D ( 'NONE', #6193, #13364, #22889 ) ;
#21552 = AXIS2_PLACEMENT_3D ( 'NONE', #13800, #12374, #4852 ) ;
#21553 = ORIENTED_EDGE ( 'NONE', *, *, #4713, .F. ) ;
#21554 = CIRCLE ( 'NONE', #6882, 4.000000000000000888 ) ;
#21555 = SHAPE_DEFINITION_REPRESENTATION ( #8356, #14072 ) ;
#21557 = ORIENTED_EDGE ( 'NONE', *, *, #5591, .F. ) ;
#21556 = ORIENTED_EDGE ( 'NONE', *, *, #7052, .F. ) ;
#21559 = ORIENTED_EDGE ( 'NONE', *, *, #7772, .T. ) ;
#21558 = ORIENTED_EDGE ( 'NONE', *, *, #14489, .F. ) ;
#21560 = CARTESIAN_POINT ( 'NONE',  ( 1.287237434361995003, 3.875615274277167455, -3.430618716627008791 ) ) ;
#21561 = CARTESIAN_POINT ( 'NONE',  ( 7.735962016526126916, -0.06991241830943736857, 7.174192622767028737 ) ) ;
#21562 =( LENGTH_UNIT ( ) NAMED_UNIT ( * ) SI_UNIT ( .MILLI., .METRE. ) );
#21563 = CIRCLE ( 'NONE', #18539, 0.5000000000000038858 ) ;
#21564 = AXIS2_PLACEMENT_3D ( 'NONE', #21431, #8945, #7186 ) ;
#21565 = DIRECTION ( 'NONE',  ( -3.885780586188016830E-16, -4.437342591868156373E-31, 1.000000000000000000 ) ) ;
#21566 = TOROIDAL_SURFACE ( 'NONE', #5003, 0.7500000000000000000, 0.2500000000000000000 ) ;
#21567 = CYLINDRICAL_SURFACE ( 'NONE', #13177, 0.5000000000000004441 ) ;
#21568 = AXIS2_PLACEMENT_3D ( 'NONE', #8697, #6699, #19391 ) ;
#21569 = CARTESIAN_POINT ( 'NONE',  ( 8.954763739086866181, -13.50000000000002309, 6.678571428571478563 ) ) ;
#21570 = CIRCLE ( 'NONE', #15167, 1.749999999999999778 ) ;
#21571 = DIRECTION ( 'NONE',  ( 0.000000000000000000, 0.000000000000000000, 1.000000000000000000 ) ) ;
#21572 = CARTESIAN_POINT ( 'NONE',  ( 5.384454397937147974, -6.874637034779069804E-15, -4.484454397937112979 ) ) ;
#21573 = DIRECTION ( 'NONE',  ( -4.615739097524200579E-16, -1.000000000000000000, -5.909321169733538150E-31 ) ) ;
#21574 = APPLICATION_CONTEXT ( 'automotive_design' ) ;
#21575 = CARTESIAN_POINT ( 'NONE',  ( 12.84999999999997300, -2.000000000000001776, 5.749999999999976907 ) ) ;
#21576 = DIRECTION ( 'NONE',  ( -0.7313537016191778983, -0.6819983600624907050, -2.183113462490731581E-16 ) ) ;
#21577 = DIRECTION ( 'NONE',  ( 4.190823558986625216E-31, -1.000000000000000000, 4.190823558986625216E-31 ) ) ;
#21578 = CARTESIAN_POINT ( 'NONE',  ( 3.999999999999955147, -3.469446951953614189E-14, 0.000000000000000000 ) ) ;
#21579 = CARTESIAN_POINT ( 'NONE',  ( 7.500000000000006217, -1.217419751680345108, 9.022398393216416679 ) ) ;
#21580 = EDGE_LOOP ( 'NONE', ( #13012, #5104, #18819, #22480 ) ) ;
#21581 = EDGE_CURVE ( 'NONE', #22262, #3520, #16887, .T. ) ;
#21582 = AXIS2_PLACEMENT_3D ( 'NONE', #11710, #8075, #4540 ) ;
#21583 = SURFACE_SIDE_STYLE ('',( #3576 ) ) ;
#21584 = CIRCLE ( 'NONE', #170, 0.5000000000000029976 ) ;
#21586 = VERTEX_POINT ( 'NONE', #20678 ) ;
#21585 = ORIENTED_EDGE ( 'NONE', *, *, #18133, .T. ) ;
#21587 = VECTOR ( 'NONE', #19006, 1000.000000000000114 ) ;
#21588 = ORIENTED_EDGE ( 'NONE', *, *, #19156, .F. ) ;
#21590 = EDGE_LOOP ( 'NONE', ( #21758, #20632, #6436, #17423 ) ) ;
#21589 = VERTEX_POINT ( 'NONE', #796 ) ;
#21591 = ORIENTED_EDGE ( 'NONE', *, *, #3625, .T. ) ;
#21592 = ORIENTED_EDGE ( 'NONE', *, *, #12844, .T. ) ;
#21593 = ORIENTED_EDGE ( 'NONE', *, *, #9415, .F. ) ;
#21594 = LINE ( 'NONE', #9107, #9566 ) ;
#21595 = SURFACE_STYLE_FILL_AREA ( #4037 ) ;
#21596 = EDGE_CURVE ( 'NONE', #7514, #9565, #1751, .T. ) ;
#21597 = DIRECTION ( 'NONE',  ( 0.000000000000000000, 0.000000000000000000, -1.000000000000000000 ) ) ;
#21598 = CARTESIAN_POINT ( 'NONE',  ( 2.918498775983380256E-10, 5.999999999003851059, -12.99999999999999822 ) ) ;
#21599 = CARTESIAN_POINT ( 'NONE',  ( 4.151274195509683906, -2.039912954708747783, -3.533232880573497159 ) ) ;
#21600 = VECTOR ( 'NONE', #13335, 1000.000000000000000 ) ;
#21601 = TOROIDAL_SURFACE ( 'NONE', #6936, 3.500000000000000000, 0.5000000000000000000 ) ;
#21602 = DIRECTION ( 'NONE',  ( 0.000000000000000000, 0.000000000000000000, -1.000000000000000000 ) ) ;
#21603 = CARTESIAN_POINT ( 'NONE',  ( -0.6810597143203314108, -4.461075778260221725, -3.598441714920940449 ) ) ;
#21604 = EDGE_CURVE ( 'NONE', #15576, #9575, #17514, .T. ) ;
#21605 = CARTESIAN_POINT ( 'NONE',  ( 3.999999999999948042, 2.309401076758532678, -5.000000000000000888 ) ) ;
#21606 = CARTESIAN_POINT ( 'NONE',  ( 66.26395429947837101, 0.000000000000000000, -5.999999999999908518 ) ) ;
#21607 = ORIENTED_EDGE ( 'NONE', *, *, #12975, .T. ) ;
#21608 = ADVANCED_FACE ( 'NONE', ( #2896 ), #1147, .F. ) ;
#21609 = CARTESIAN_POINT ( 'NONE',  ( 0.000000000000000000, 1.750000000000001554, 0.000000000000000000 ) ) ;
#21611 = ORIENTED_EDGE ( 'NONE', *, *, #13106, .T. ) ;
#21610 = ORIENTED_EDGE ( 'NONE', *, *, #13244, .F. ) ;
#21612 = B_SPLINE_CURVE_WITH_KNOTS ( 'NONE', 3,
 ( #2254, #4012, #9553, #5683 ),
 .UNSPECIFIED., .F., .F.,
 ( 4, 4 ),
 ( 0.000000000000000000, 0.002452478801916372839 ),
 .UNSPECIFIED. ) ;
#21613 = ADVANCED_FACE ( 'NONE', ( #22670 ), #20169, .T. ) ;
#21614 = EDGE_LOOP ( 'NONE', ( #18500, #12597 ) ) ;
#21615 = AXIS2_PLACEMENT_3D ( 'NONE', #16120, #22856, #3559 ) ;
#21616 = ADVANCED_FACE ( 'NONE', ( #4772 ), #11943, .F. ) ;
#21617 = ORIENTED_EDGE ( 'NONE', *, *, #21894, .T. ) ;
#21618 = VERTEX_POINT ( 'NONE', #21261 ) ;
#21619 = ADVANCED_FACE ( 'NONE', ( #17954 ), #2490, .T. ) ;
#21620 = ORIENTED_EDGE ( 'NONE', *, *, #11370, .F. ) ;
#21621 = CARTESIAN_POINT ( 'NONE',  ( 6.999999999999978684, -5.999999999999981348, 11.74999999999998224 ) ) ;
#21622 = DIRECTION ( 'NONE',  ( 1.333893503340774882E-15, 2.778352770573747380E-17, 1.000000000000000000 ) ) ;
#21623 = LINE ( 'NONE', #17611, #8522 ) ;
#21624 = CARTESIAN_POINT ( 'NONE',  ( 10.49999999999998224, 0.000000000000000000, 5.750000000000005329 ) ) ;
#21625 = DIRECTION ( 'NONE',  ( 1.454462294001240516E-30, 1.000000000000000000, 0.000000000000000000 ) ) ;
#21626 = CARTESIAN_POINT ( 'NONE',  ( -6.000000000000074607, -4.800000000000026468, -7.500000000000034639 ) ) ;
#21627 = DIRECTION ( 'NONE',  ( -1.000000000000000000, 1.847414967615758933E-47, -3.885780586188017323E-16 ) ) ;
#21628 = DIRECTION ( 'NONE',  ( 0.7313537016191733464, -0.6819983600624954789, 3.733258675956564523E-18 ) ) ;
#21629 = EDGE_CURVE ( 'NONE', #1104, #6270, #17920, .T. ) ;
#21630 = ADVANCED_FACE ( 'NONE', ( #3479 ), #1595, .T. ) ;
#21631 = CARTESIAN_POINT ( 'NONE',  ( -7.568268608012067133, -13.53268520232740357, 8.579161250779877790 ) ) ;
#21632 = CONICAL_SURFACE ( 'NONE', #1704, 4.000000000000000000, 1.047197551196595855 ) ;
#21633 = EDGE_CURVE ( 'NONE', #19696, #8999, #14154, .T. ) ;
#21634 = LINE ( 'NONE', #7386, #15313 ) ;
#21635 = AXIS2_PLACEMENT_3D ( 'NONE', #19287, #7066, #8701 ) ;
#21636 = DIRECTION ( 'NONE',  ( -8.438582421954109416E-32, 0.000000000000000000, -1.000000000000000000 ) ) ;
#21637 = CARTESIAN_POINT ( 'NONE',  ( 36.00000000029184832, 16.99999999900385461, -25.50000000000000355 ) ) ;
#21638 = CARTESIAN_POINT ( 'NONE',  ( 8.954763739086851970, -1.500000000000001332, 6.678571428571422608 ) ) ;
#21639 = DIRECTION ( 'NONE',  ( 1.066811114794976679E-26, 0.000000000000000000, 1.000000000000000000 ) ) ;
#21640 = FACE_OUTER_BOUND ( 'NONE', #6448, .T. ) ;
#21641 = ORIENTED_EDGE ( 'NONE', *, *, #17447, .T. ) ;
#21642 = ADVANCED_FACE ( 'NONE', ( #5126 ), #6900, .T. ) ;
#21643 = EDGE_CURVE ( 'NONE', #3351, #20629, #20496, .T. ) ;
#21644 = VERTEX_POINT ( 'NONE', #21019 ) ;
#21645 = DIRECTION ( 'NONE',  ( 2.013525853228507892E-32, 6.902532920683810383E-31, -1.000000000000000000 ) ) ;
#21646 = ORIENTED_EDGE ( 'NONE', *, *, #14102, .T. ) ;
#21647 = CARTESIAN_POINT ( 'NONE',  ( 3.522875095018858094, -2.820352903224746743, -3.598441714920217471 ) ) ;
#21648 = CARTESIAN_POINT ( 'NONE',  ( -4.750000000000000000, 3.766740792898668295E-14, -3.733602117766605407E-17 ) ) ;
#21649 = CARTESIAN_POINT ( 'NONE',  ( 8.697224362267997222, -12.00000000000002842, 6.250000000000019540 ) ) ;
#21650 = DIRECTION ( 'NONE',  ( 3.885780586188016830E-16, 4.437342591868156373E-31, -1.000000000000000000 ) ) ;
#21651 = ORIENTED_EDGE ( 'NONE', *, *, #13844, .F. ) ;
#21652 = VECTOR ( 'NONE', #10261, 1000.000000000000000 ) ;
#21653 = DIRECTION ( 'NONE',  ( 0.000000000000000000, -1.000000000000000000, 0.000000000000000000 ) ) ;
#21654 = DIRECTION ( 'NONE',  ( 0.000000000000000000, 0.000000000000000000, 1.000000000000000000 ) ) ;
#21655 = CARTESIAN_POINT ( 'NONE',  ( 0.000000000000000000, 0.000000000000000000, -3.499999999999996003 ) ) ;
#21656 = CARTESIAN_POINT ( 'NONE',  ( -6.961281259571826752, 35.99999999900384751, -18.51954822859009653 ) ) ;
#21657 = VECTOR ( 'NONE', #9525, 1000.000000000000000 ) ;
#21658 = CARTESIAN_POINT ( 'NONE',  ( -6.999999999708142795, 36.49999999900384751, -19.50000000000000355 ) ) ;
#21659 = DIRECTION ( 'NONE',  ( 0.7071067811865475727, -0.7071067811865475727, 0.000000000000000000 ) ) ;
#21660 = DIRECTION ( 'NONE',  ( 1.000000000000000000, 2.168404344970995063E-16, 0.000000000000000000 ) ) ;
#21661 = CARTESIAN_POINT ( 'NONE',  ( -55.25320565519145788, -4.163336342344337027E-14, 10.00000000000009237 ) ) ;
#21662 = CARTESIAN_POINT ( 'NONE',  ( -89.70000000000064233, 5.551115123125782702E-14, -2.000000000000001776 ) ) ;
#21663 = ADVANCED_FACE ( 'NONE', ( #3379, #16165 ), #83, .F. ) ;
#21664 = VERTEX_POINT ( 'NONE', #16049 ) ;
#21665 = APPLICATION_PROTOCOL_DEFINITION ( 'draft international standard', 'automotive_design', 1998, #2311 ) ;
#21666 = EDGE_CURVE ( 'NONE', #14655, #2319, #14071, .T. ) ;
#21668 = ORIENTED_EDGE ( 'NONE', *, *, #18570, .F. ) ;
#21667 = ORIENTED_EDGE ( 'NONE', *, *, #9405, .T. ) ;
#21669 = ADVANCED_FACE ( 'NONE', ( #23260 ), #10536, .F. ) ;
#21670 = EDGE_LOOP ( 'NONE', ( #18918, #22408, #15542, #753 ) ) ;
#21672 = VERTEX_POINT ( 'NONE', #7251 ) ;
#21671 = ORIENTED_EDGE ( 'NONE', *, *, #1723, .T. ) ;
#21673 = CARTESIAN_POINT ( 'NONE',  ( 3.540020015735602765, 2.810662092923783550, -3.602146406945765822 ) ) ;
#21674 = DIRECTION ( 'NONE',  ( 0.000000000000000000, 0.000000000000000000, -1.000000000000000000 ) ) ;
#21675 = CARTESIAN_POINT ( 'NONE',  ( 7.523705677365021494, -11.16164950473969775, 8.715168381946160281 ) ) ;
#21676 = CARTESIAN_POINT ( 'NONE',  ( -12.84999999999999964, -12.50000000000006928, 6.938893903907228378E-14 ) ) ;
#21677 = EDGE_CURVE ( 'NONE', #17626, #20741, #16751, .T. ) ;
#21678 = DIRECTION ( 'NONE',  ( -1.066786462891689527E-26, -6.656013887802287108E-31, -1.000000000000000000 ) ) ;
#21679 = DIRECTION ( 'NONE',  ( 0.000000000000000000, -1.000000000000000000, 0.000000000000000000 ) ) ;
#21680 = DIRECTION ( 'NONE',  ( 0.000000000000000000, -1.000000000000000000, 0.000000000000000000 ) ) ;
#21681 = DIRECTION ( 'NONE',  ( -1.000000000000000000, 1.776356839400250465E-15, 0.000000000000000000 ) ) ;
#21682 = AXIS2_PLACEMENT_3D ( 'NONE', #6574, #1163, #13853 ) ;
#21683 = CARTESIAN_POINT ( 'NONE',  ( 0.000000000000000000, 2.775557561562891351E-14, 17.49999999999997513 ) ) ;
#21684 = CYLINDRICAL_SURFACE ( 'NONE', #10294, 3.000000000000011102 ) ;
#21685 = DIRECTION ( 'NONE',  ( -0.000000000000000000, -1.000000000000000000, -0.000000000000000000 ) ) ;
#21686 = AXIS2_PLACEMENT_3D ( 'NONE', #15905, #8515, #3349 ) ;
#21687 = CARTESIAN_POINT ( 'NONE',  ( 37.00000000000014211, 10.75000000000000000, -2.566987298107808790 ) ) ;
#21688 = DIRECTION ( 'NONE',  ( -3.885780586188016830E-16, -4.437342591868156373E-31, 1.000000000000000000 ) ) ;
#21689 = B_SPLINE_CURVE_WITH_KNOTS ( 'NONE', 3,
 ( #1586, #19353, #3250, #8766, #10412, #7702, #7244, #9582 ),
 .UNSPECIFIED., .F., .F.,
 ( 4, 2, 2, 4 ),
 ( 0.000000000000000000, 0.002450665683189822731, 0.003675998524784734097, 0.004901331366379645463 ),
 .UNSPECIFIED. ) ;
#21690 = DIRECTION ( 'NONE',  ( 3.032184104443272185E-30, 1.000000000000000000, -7.395570986447005381E-32 ) ) ;
#21691 = CARTESIAN_POINT ( 'NONE',  ( 8.510464245293309915, -0.5071972189929013775, 6.988717072694006660 ) ) ;
#21692 = ORIENTED_EDGE ( 'NONE', *, *, #3222, .F. ) ;
#21694 = ORIENTED_EDGE ( 'NONE', *, *, #7359, .F. ) ;
#21693 = ORIENTED_EDGE ( 'NONE', *, *, #4722, .T. ) ;
#21695 = ORIENTED_EDGE ( 'NONE', *, *, #20327, .T. ) ;
#21697 = VERTEX_POINT ( 'NONE', #5004 ) ;
#21696 = VERTEX_POINT ( 'NONE', #15936 ) ;
#21698 = VECTOR ( 'NONE', #13967, 1000.000000000000000 ) ;
#21699 = ORIENTED_EDGE ( 'NONE', *, *, #21108, .F. ) ;
#21700 = CARTESIAN_POINT ( 'NONE',  ( 4.158413352280801334, 2.044871626972824430, 3.541821552872959966 ) ) ;
#21701 = AXIS2_PLACEMENT_3D ( 'NONE', #14456, #1517, #5041 ) ;
#21702 = EDGE_LOOP ( 'NONE', ( #2648, #3747, #8003, #17688 ) ) ;
#21703 = ORIENTED_EDGE ( 'NONE', *, *, #17121, .F. ) ;
#21704 = FACE_OUTER_BOUND ( 'NONE', #22500, .T. ) ;
#21705 = CARTESIAN_POINT ( 'NONE',  ( 0.000000000000000000, 2.775557561562891351E-14, 17.49999999999997513 ) ) ;
#21706 = DIRECTION ( 'NONE',  ( -1.000000000000000000, -2.220446049250313081E-16, 0.000000000000000000 ) ) ;
#21707 = DIRECTION ( 'NONE',  ( 0.000000000000000000, 0.000000000000000000, -1.000000000000000000 ) ) ;
#21708 = EDGE_CURVE ( 'NONE', #10595, #7934, #19781, .T. ) ;
#21709 = VECTOR ( 'NONE', #5100, 1000.000000000000000 ) ;
#21710 = DIRECTION ( 'NONE',  ( -1.000000000000000000, -4.440892098500626162E-16, 5.551115123125782702E-16 ) ) ;
#21711 = CARTESIAN_POINT ( 'NONE',  ( 112.6756160111034006, -11.28140466348826010, 6.000000000000032863 ) ) ;
#21712 = CARTESIAN_POINT ( 'NONE',  ( -4.175002511812232697, -2.208363329454933410, -3.469254087858270719 ) ) ;
#21713 = SURFACE_SIDE_STYLE ('',( #17946 ) ) ;
#21714 = CARTESIAN_POINT ( 'NONE',  ( 119.5756419024615269, -4.000000000000058620, -5.999999999999984901 ) ) ;
#21715 = FACE_OUTER_BOUND ( 'NONE', #10543, .T. ) ;
#21716 = VECTOR ( 'NONE', #944, 1000.000000000000000 ) ;
#21717 = CARTESIAN_POINT ( 'NONE',  ( -6.000000000000088818, -2.000000000000043521, 7.500000000000076383 ) ) ;
#21718 = AXIS2_PLACEMENT_3D ( 'NONE', #1121, #9815, #13701 ) ;
#21719 = EDGE_LOOP ( 'NONE', ( #13503, #18078, #16254, #5786 ) ) ;
#21720 = PRESENTATION_STYLE_ASSIGNMENT (( #7590 ) ) ;
#21721 = CARTESIAN_POINT ( 'NONE',  ( 108.2426266706970637, -6.527605602963671316, -5.999999999999991118 ) ) ;
#21723 = EDGE_LOOP ( 'NONE', ( #18532, #17213, #22412, #1402 ) ) ;
#21722 = VERTEX_POINT ( 'NONE', #23141 ) ;
#21724 = AXIS2_PLACEMENT_3D ( 'NONE', #15982, #3419, #12457 ) ;
#21725 = VERTEX_POINT ( 'NONE', #10991 ) ;
#21726 = VERTEX_POINT ( 'NONE', #20177 ) ;
#21727 = ORIENTED_EDGE ( 'NONE', *, *, #5798, .F. ) ;
#21728 = EDGE_LOOP ( 'NONE', ( #3384, #22034, #22178 ) ) ;
#21729 = EDGE_LOOP ( 'NONE', ( #8899, #18493, #181, #5610 ) ) ;
#21730 = DIRECTION ( 'NONE',  ( -5.551115123561405253E-17, -1.000000000000000000, -2.256980353643891447E-27 ) ) ;
#21731 = PRESENTATION_LAYER_ASSIGNMENT (  '', '', ( #13466 ) ) ;
#21732 = CARTESIAN_POINT ( 'NONE',  ( 4.175813232069142344, 2.061359961916371830, 3.570380186727395433 ) ) ;
#21733 = ADVANCED_FACE ( 'NONE', ( #2054 ), #20065, .F. ) ;
#21734 = CARTESIAN_POINT ( 'NONE',  ( -0.3198814748698700083, -4.434118497892228561, -0.3507732604232856044 ) ) ;
#21735 = CARTESIAN_POINT ( 'NONE',  ( -43.46238456605044576, 4.919238815542528620, 7.500000000000034639 ) ) ;
#21736 = CONICAL_SURFACE ( 'NONE', #14591, 4.000000000000000000, 1.047197551196595855 ) ;
#21737 = CARTESIAN_POINT ( 'NONE',  ( 8.391189084741249360, -12.47320284813923585, 7.111621047081361446 ) ) ;
#21738 = CARTESIAN_POINT ( 'NONE',  ( -89.70000000000057128, -9.020562075079396891E-14, -2.000000000000001776 ) ) ;
#21739 = CARTESIAN_POINT ( 'NONE',  ( -8.697224362267997222, -1.999999999999998224, 6.249999999999977796 ) ) ;
#21740 = CIRCLE ( 'NONE', #19107, 2.499999999999990674 ) ;
#21741 = FACE_OUTER_BOUND ( 'NONE', #3849, .T. ) ;
#21742 = ADVANCED_FACE ( 'NONE', ( #300 ), #14902, .T. ) ;
#21743 = VECTOR ( 'NONE', #2108, 1000.000000000000000 ) ;
#21744 = VECTOR ( 'NONE', #12403, 1000.000000000000000 ) ;
#21745 = EDGE_CURVE ( 'NONE', #21501, #16094, #9467, .T. ) ;
#21746 = CARTESIAN_POINT ( 'NONE',  ( 124.5000000000017195, -4.000000000000058620, 1.387778780781445676E-14 ) ) ;
#21747 = DIRECTION ( 'NONE',  ( -4.019602852144232182E-47, -6.982962677686261977E-15, -1.000000000000000000 ) ) ;
#21749 = EDGE_CURVE ( 'NONE', #17392, #11726, #10025, .T. ) ;
#21748 = CARTESIAN_POINT ( 'NONE',  ( 37.54332536350041494, 0.1155932590976401775, -10.22062532321603712 ) ) ;
#21750 = DIRECTION ( 'NONE',  ( 5.551115123561405253E-17, 1.000000000000000000, 2.256980353643891447E-27 ) ) ;
#21751 = DIRECTION ( 'NONE',  ( 2.220446049250313081E-16, -1.000000000000000000, 7.025792437124636392E-31 ) ) ;
#21752 = EDGE_LOOP ( 'NONE', ( #21440, #10885, #21592, #2766 ) ) ;
#21753 = ORIENTED_EDGE ( 'NONE', *, *, #12427, .T. ) ;
#21754 = DIRECTION ( 'NONE',  ( 0.000000000000000000, 0.000000000000000000, 1.000000000000000000 ) ) ;
#21755 = EDGE_CURVE ( 'NONE', #1743, #22996, #2170, .T. ) ;
#21756 = AXIS2_PLACEMENT_3D ( 'NONE', #17913, #9079, #5324 ) ;
#21757 = FACE_OUTER_BOUND ( 'NONE', #4141, .T. ) ;
#21758 = ORIENTED_EDGE ( 'NONE', *, *, #1959, .F. ) ;
#21759 = DIRECTION ( 'NONE',  ( -1.000000000000000000, 4.190823558986610327E-31, -1.733449886265890494E-32 ) ) ;
#21760 = DIRECTION ( 'NONE',  ( -1.000000000000000000, 1.550910762415513985E-16, 3.012982189080959477E-32 ) ) ;
#21761 = DIRECTION ( 'NONE',  ( 3.885780586188016830E-16, 4.437342591868156373E-31, -1.000000000000000000 ) ) ;
#21762 = DIRECTION ( 'NONE',  ( -0.000000000000000000, -0.000000000000000000, 1.000000000000000000 ) ) ;
#21763 = EDGE_LOOP ( 'NONE', ( #8870, #3268, #1607, #19415 ) ) ;
#21764 = DIRECTION ( 'NONE',  ( 0.000000000000000000, 0.000000000000000000, 1.000000000000000000 ) ) ;
#21765 = CARTESIAN_POINT ( 'NONE',  ( 54.42435809754106657, -4.000000000000003553, 6.000000000000136779 ) ) ;
#21766 = ADVANCED_FACE ( 'NONE', ( #3816 ), #13000, .F. ) ;
#21767 = CARTESIAN_POINT ( 'NONE',  ( 29.00000000029184832, 16.99999999900385461, -15.99999999999999289 ) ) ;
#21768 = CARTESIAN_POINT ( 'NONE',  ( -6.962001439796694058, 35.99999999900384751, -18.52402997057235723 ) ) ;
#21769 = CARTESIAN_POINT ( 'NONE',  ( 7.604097569491849562, -13.58924811263090326, 8.440516644273110103 ) ) ;
#21770 = CARTESIAN_POINT ( 'NONE',  ( -6.000000000000130562, 1.999999999999960032, -8.000000000000035527 ) ) ;
#21771 = EDGE_CURVE ( 'NONE', #888, #3083, #7588, .T. ) ;
#21772 = CARTESIAN_POINT ( 'NONE',  ( 56.00000000000088107, 0.000000000000000000, 6.500000000000117240 ) ) ;
#21773 = CARTESIAN_POINT ( 'NONE',  ( 3.951447005078449148, -1.347150628109124559, -3.500000000000001332 ) ) ;
#21775 = EDGE_CURVE ( 'NONE', #21498, #10194, #15634, .T. ) ;
#21774 = CARTESIAN_POINT ( 'NONE',  ( 114.8016533820239005, -4.500000000000059508, -5.999999999999984901 ) ) ;
#21776 = AXIS2_PLACEMENT_3D ( 'NONE', #9591, #12883, #542 ) ;
#21777 = DIRECTION ( 'NONE',  ( -0.8660254037844387076, 2.506296930348934952E-16, 0.4999999999999999445 ) ) ;
#21778 = VECTOR ( 'NONE', #7494, 1000.000000000000000 ) ;
#21779 = SHAPE_DEFINITION_REPRESENTATION ( #4390, #1856 ) ;
#21780 = VECTOR ( 'NONE', #20714, 1000.000000000000000 ) ;
#21782 = EDGE_LOOP ( 'NONE', ( #12148, #12737 ) ) ;
#21781 = ORIENTED_EDGE ( 'NONE', *, *, #12553, .T. ) ;
#21783 = PRODUCT_DEFINITION_FORMATION_WITH_SPECIFIED_SOURCE ( 'ANY', '', #20565, .NOT_KNOWN. ) ;
#21784 = ORIENTED_EDGE ( 'NONE', *, *, #15556, .F. ) ;
#21785 = EDGE_CURVE ( 'NONE', #7514, #21116, #20295, .T. ) ;
#21787 = VERTEX_POINT ( 'NONE', #11332 ) ;
#21786 = ORIENTED_EDGE ( 'NONE', *, *, #1487, .F. ) ;
#21788 = DIRECTION ( 'NONE',  ( 1.000000000000000000, -7.100545512326564696E-57, -1.066786462891689527E-26 ) ) ;
#21789 = CARTESIAN_POINT ( 'NONE',  ( 37.69160037009711317, 0.02335407096321897094, -2.482824663591205461 ) ) ;
#21790 = CARTESIAN_POINT ( 'NONE',  ( 7.901093513163756299, -12.32682690073933252, 7.745538272134628421 ) ) ;
#21791 = CARTESIAN_POINT ( 'NONE',  ( -43.10883117545713361, -4.565685424949242233, 8.000000000000035527 ) ) ;
#21792 = ADVANCED_FACE ( 'NONE', ( #18519 ), #13030, .T. ) ;
#21793 = DIRECTION ( 'NONE',  ( 0.000000000000000000, 0.000000000000000000, 1.000000000000000000 ) ) ;
#21794 = CARTESIAN_POINT ( 'NONE',  ( 0.000000000000000000, 0.000000000000000000, -4.974599999999998801 ) ) ;
#21795 = CARTESIAN_POINT ( 'NONE',  ( -6.958039891257955745, 36.00029345514013102, -18.49999999999999645 ) ) ;
#21796 = CARTESIAN_POINT ( 'NONE',  ( 0.000000000000000000, 0.000000000000000000, 0.000000000000000000 ) ) ;
#21797 = CARTESIAN_POINT ( 'NONE',  ( -45.91923881554284037, 2.462384566050156209, 8.000000000000076383 ) ) ;
#21798 = CARTESIAN_POINT ( 'NONE',  ( 108.2426266706970353, -13.52760560296359316, -6.000000000000019540 ) ) ;
#21799 = VECTOR ( 'NONE', #22162, 1000.000000000000000 ) ;
#21800 = DIRECTION ( 'NONE',  ( -9.693457064947022734E-26, 0.000000000000000000, 1.000000000000000000 ) ) ;
#21801 = LINE ( 'NONE', #12489, #9483 ) ;
#21802 = VERTEX_POINT ( 'NONE', #15537 ) ;
#21803 = CARTESIAN_POINT ( 'NONE',  ( 0.000000000000000000, 0.000000000000000000, 0.000000000000000000 ) ) ;
#21804 = CARTESIAN_POINT ( 'NONE',  ( 7.761744141695581689, -2.064358047808337204, 6.973942750959555958 ) ) ;
#21805 = CARTESIAN_POINT ( 'NONE',  ( 22.49999999999996092, 2.000000000000043521, -17.50000000000001066 ) ) ;
#21806 = PLANE ( 'NONE',  #6281 ) ;
#21807 = EDGE_LOOP ( 'NONE', ( #16516, #7477, #9305, #21209 ) ) ;
#21809 = ORIENTED_EDGE ( 'NONE', *, *, #8180, .F. ) ;
#21808 = ORIENTED_EDGE ( 'NONE', *, *, #17567, .T. ) ;
#21810 = ORIENTED_EDGE ( 'NONE', *, *, #557, .F. ) ;
#21811 = ORIENTED_EDGE ( 'NONE', *, *, #1770, .F. ) ;
#21813 = EDGE_LOOP ( 'NONE', ( #3458, #1383, #19539, #19218 ) ) ;
#21812 = ORIENTED_EDGE ( 'NONE', *, *, #1485, .F. ) ;
#21814 = AXIS2_PLACEMENT_3D ( 'NONE', #7105, #4849, #20978 ) ;
#21815 = VERTEX_POINT ( 'NONE', #5484 ) ;
#21816 = LINE ( 'NONE', #18275, #20402 ) ;
#21817 = ORIENTED_EDGE ( 'NONE', *, *, #5351, .T. ) ;
#21818 = ORIENTED_EDGE ( 'NONE', *, *, #14570, .F. ) ;
#21819 = DIRECTION ( 'NONE',  ( -1.000000000000000000, 2.785515554063903297E-14, 1.815210279346915817E-30 ) ) ;
#21820 = SURFACE_SIDE_STYLE ('',( #21595 ) ) ;
#21821 = EDGE_CURVE ( 'NONE', #12647, #19572, #194, .T. ) ;
#21822 = DIRECTION ( 'NONE',  ( -2.775557561562887961E-17, 2.857733511404945646E-16, -1.000000000000000000 ) ) ;
#21823 = CARTESIAN_POINT ( 'NONE',  ( 0.000000000000000000, 0.000000000000000000, 0.000000000000000000 ) ) ;
#21824 = LINE ( 'NONE', #5710, #13633 ) ;
#21825 = CARTESIAN_POINT ( 'NONE',  ( 2.742413778650823364, 1.325747111984056037, -4.750000000000000888 ) ) ;
#21826 = DIRECTION ( 'NONE',  ( 1.331202777560457422E-30, 1.000000000000000000, -7.395570986446985676E-31 ) ) ;
#21827 = DIRECTION ( 'NONE',  ( -3.944304526105059027E-31, -6.383782391594650107E-16, -1.000000000000000000 ) ) ;
#21828 = EDGE_CURVE ( 'NONE', #6591, #20837, #11455, .T. ) ;
#21829 = CARTESIAN_POINT ( 'NONE',  ( 7.949747468597695210, 47.94974746730969173, -25.50000000000000355 ) ) ;
#21830 = VECTOR ( 'NONE', #19767, 1000.000000000000000 ) ;
#21831 = CARTESIAN_POINT ( 'NONE',  ( 37.34641016151397253, 10.60000000000007958, -2.653589838486262398 ) ) ;
#21832 = ORIENTED_EDGE ( 'NONE', *, *, #4981, .T. ) ;
#21833 = DIRECTION ( 'NONE',  ( -1.000000000000000000, -2.699383410053119644E-30, -3.330669073875432643E-16 ) ) ;
#21835 = ORIENTED_EDGE ( 'NONE', *, *, #6624, .F. ) ;
#21834 = ORIENTED_EDGE ( 'NONE', *, *, #16401, .F. ) ;
#21836 = B_SPLINE_CURVE_WITH_KNOTS ( 'NONE', 3,
 ( #7528, #21996, #14690, #20112, #9522, #16678 ),
 .UNSPECIFIED., .F., .F.,
 ( 4, 2, 4 ),
 ( 0.002044882221487528875, 0.003063384235218492846, 0.004081886248949457251 ),
 .UNSPECIFIED. ) ;
#21837 = ORIENTED_EDGE ( 'NONE', *, *, #8635, .F. ) ;
#21838 = ORIENTED_EDGE ( 'NONE', *, *, #3507, .T. ) ;
#21839 = CARTESIAN_POINT ( 'NONE',  ( 30.00000000029184832, 2.999999999003851503, -5.999999999999998224 ) ) ;
#21840 = CIRCLE ( 'NONE', #802, 2.550000000000024691 ) ;
#21841 = TOROIDAL_SURFACE ( 'NONE', #15445, 6.000000000000015987, 0.5000000000000000000 ) ;
#21842 = FACE_OUTER_BOUND ( 'NONE', #339, .T. ) ;
#21843 = CARTESIAN_POINT ( 'NONE',  ( 4.165266963751727225, -2.049631966911992897, -3.550066703508901078 ) ) ;
#21844 = CARTESIAN_POINT ( 'NONE',  ( 25.15499999999999403, 3.061616997868413710E-16, -2.500000000000007550 ) ) ;
#21845 = LINE ( 'NONE', #16524, #345 ) ;
#21846 = CARTESIAN_POINT ( 'NONE',  ( 8.715898959466901630, -12.49756837761076333, 6.833978265954070430 ) ) ;
#21847 = CARTESIAN_POINT ( 'NONE',  ( 61.83096495907209089, -4.753799060524588782, 6.500000000000179412 ) ) ;
#21848 = DIRECTION ( 'NONE',  ( 3.885780586188016830E-16, 4.437342591868156373E-31, -1.000000000000000000 ) ) ;
#21849 = CARTESIAN_POINT ( 'NONE',  ( -42.54314575050793934, 3.999999999999996447, 7.500000000000062172 ) ) ;
#21850 = CARTESIAN_POINT ( 'NONE',  ( -10.49999999999998224, -14.00000000000003020, 6.250000000000033751 ) ) ;
#21851 = FACE_OUTER_BOUND ( 'NONE', #14968, .T. ) ;
#21852 = DIRECTION ( 'NONE',  ( 1.733449886265891589E-32, -4.190823558986610327E-31, 1.000000000000000000 ) ) ;
#21853 = PRODUCT_DEFINITION ( 'UNKNOWN', '', #759, #2056 ) ;
#21854 = LINE ( 'NONE', #5748, #14227 ) ;
#21856 = AXIS2_PLACEMENT_3D ( 'NONE', #14065, #3253, #4998 ) ;
#21855 = DIRECTION ( 'NONE',  ( 2.013525853228518840E-32, -6.902532920683810383E-31, 1.000000000000000000 ) ) ;
#21857 = AXIS2_PLACEMENT_3D ( 'NONE', #19979, #14909, #21861 ) ;
#21858 = EDGE_CURVE ( 'NONE', #7622, #8200, #5889, .T. ) ;
#21859 = ORIENTED_EDGE ( 'NONE', *, *, #22185, .F. ) ;
#21860 = CARTESIAN_POINT ( 'NONE',  ( -6.525612274168519633, 36.03379296756838812, -27.63750043262194112 ) ) ;
#21861 = DIRECTION ( 'NONE',  ( 1.000000000000000000, 0.000000000000000000, 0.000000000000000000 ) ) ;
#21863 = ADVANCED_FACE ( 'NONE', ( #18758 ), #7933, .F. ) ;
#21862 = ORIENTED_EDGE ( 'NONE', *, *, #18052, .T. ) ;
#21864 =( REPRESENTATION_RELATIONSHIP ('NONE','NONE', #19450, #1164 ) REPRESENTATION_RELATIONSHIP_WITH_TRANSFORMATION ( #7878 )SHAPE_REPRESENTATION_RELATIONSHIP( ) );
#21865 = LINE ( 'NONE', #22217, #22648 ) ;
#21866 = CARTESIAN_POINT ( 'NONE',  ( -89.70000000000064233, 3.200000000000057021, -2.000000000000001776 ) ) ;
#21867 = CARTESIAN_POINT ( 'NONE',  ( 3.973514160553471619, 3.435084588004206019, -1.181876024140340986 ) ) ;
#21868 = CARTESIAN_POINT ( 'NONE',  ( 86.00000000000133582, -13.02760560296348302, -5.999999999999956479 ) ) ;
#21869 = CARTESIAN_POINT ( 'NONE',  ( 2.661839581153344325E-13, 4.796734841935159643, -3.721909803043225828 ) ) ;
#21870 = CARTESIAN_POINT ( 'NONE',  ( -91.02295700146262902, 3.200000000000015277, 6.338518968055040226 ) ) ;
#21871 = AXIS2_PLACEMENT_3D ( 'NONE', #15930, #14949, #16580 ) ;
#21872 = DIRECTION ( 'NONE',  ( -1.000000000000000000, -1.700709290173333260E-16, 0.000000000000000000 ) ) ;
#21873 = CARTESIAN_POINT ( 'NONE',  ( 8.660254037844413944, 4.689110867544616035, 2.775557561562891351E-14 ) ) ;
#21874 = VECTOR ( 'NONE', #9890, 1000.000000000000000 ) ;
#21875 = CARTESIAN_POINT ( 'NONE',  ( 3.951447005078449148, 1.347150628109116566, 3.499999999999997335 ) ) ;
#21876 = DIRECTION ( 'NONE',  ( 1.000000000000000000, 1.600676661924044152E-14, 0.000000000000000000 ) ) ;
#21877 = DIRECTION ( 'NONE',  ( 1.734723475976805517E-15, -1.000000000000000000, 0.000000000000000000 ) ) ;
#21878 = LINE ( 'NONE', #14692, #21925 ) ;
#21879 = CARTESIAN_POINT ( 'NONE',  ( -95.20000000000065654, -0.5000000000000975886, -2.000000000000001776 ) ) ;
#21880 = ADVANCED_FACE ( 'NONE', ( #6181 ), #15091, .F. ) ;
#21881 = CARTESIAN_POINT ( 'NONE',  ( 4.175572532730925879, 2.061029303918053390, -3.569807470274388717 ) ) ;
#21882 = EDGE_CURVE ( 'NONE', #21725, #6467, #22404, .T. ) ;
#21883 = PRODUCT_CONTEXT ( 'NONE', #2628, 'mechanical' ) ;
#21884 = CIRCLE ( 'NONE', #15494, 5.500000000000032863 ) ;
#21885 = EDGE_LOOP ( 'NONE', ( #4309, #10834, #20386, #18387, #5313, #15793 ) ) ;
#21886 = AXIS2_PLACEMENT_3D ( 'NONE', #8561, #15724, #19374 ) ;
#21887 = VECTOR ( 'NONE', #20202, 1000.000000000000000 ) ;
#21888 = VECTOR ( 'NONE', #6096, 1000.000000000000000 ) ;
#21891 = VERTEX_POINT ( 'NONE', #18869 ) ;
#21890 = ADVANCED_FACE ( 'NONE', ( #17323 ), #2871, .T. ) ;
#21889 = ORIENTED_EDGE ( 'NONE', *, *, #11979, .T. ) ;
#21892 = EDGE_CURVE ( 'NONE', #7256, #20837, #8916, .T. ) ;
#21893 = DIRECTION ( 'NONE',  ( -1.000000000000000000, -1.479114197289388027E-30, -2.013525853228507892E-32 ) ) ;
#21894 = EDGE_CURVE ( 'NONE', #9575, #9299, #22287, .T. ) ;
#21895 = CARTESIAN_POINT ( 'NONE',  ( 7.126417736726676999, -0.4330224014298832969, 8.494066294656319016 ) ) ;
#21896 = CARTESIAN_POINT ( 'NONE',  ( 8.260108127873353467, -11.89083139210928408, 7.249251683976535077 ) ) ;
#21897 = ORIENTED_EDGE ( 'NONE', *, *, #7266, .F. ) ;
#21898 = CARTESIAN_POINT ( 'NONE',  ( 88.75737332930596324, -13.52760560296348302, -6.499999999999964473 ) ) ;
#21899 = CARTESIAN_POINT ( 'NONE',  ( -5.710259475508905133E-15, -22.91099746826335348, -10.34816708862278212 ) ) ;
#21900 = DIRECTION ( 'NONE',  ( -7.160938508832258108E-15, 0.000000000000000000, 1.000000000000000000 ) ) ;
#21901 = CARTESIAN_POINT ( 'NONE',  ( -3.999999999708153453, 38.99999999900385461, -15.99999999999999289 ) ) ;
#21902 = CARTESIAN_POINT ( 'NONE',  ( -1.321505333908965962, 3.855830693249139962, -5.565789719053468865 ) ) ;
#21903 = CARTESIAN_POINT ( 'NONE',  ( -45.37157287525410254, -6.828427124746225374, 8.000000000000035527 ) ) ;
#21904 = DIRECTION ( 'NONE',  ( 1.733449886265891589E-32, -4.190823558986610327E-31, 1.000000000000000000 ) ) ;
#21905 = AXIS2_PLACEMENT_3D ( 'NONE', #5796, #11416, #20257 ) ;
#21906 = FACE_OUTER_BOUND ( 'NONE', #22656, .T. ) ;
#21907 = CIRCLE ( 'NONE', #22668, 6.700000000000039257 ) ;
#21908 = PRESENTATION_STYLE_ASSIGNMENT (( #14719 ) ) ;
#21909 = CONICAL_SURFACE ( 'NONE', #9132, 2.055000000000002380, 0.7853981633974400633 ) ;
#21910 = DIRECTION ( 'NONE',  ( -9.693457064947022734E-26, 0.000000000000000000, 1.000000000000000000 ) ) ;
#21911 = ADVANCED_FACE ( 'NONE', ( #13582 ), #7607, .F. ) ;
#21912 = TOROIDAL_SURFACE ( 'NONE', #11754, 2.250000000000000444, 0.2500000000000000000 ) ;
#21914 = EDGE_CURVE ( 'NONE', #4310, #7880, #4773, .T. ) ;
#21913 = DIRECTION ( 'NONE',  ( 1.000000000000000000, 0.000000000000000000, 2.668805347656595124E-16 ) ) ;
#21915 = ADVANCED_FACE ( 'NONE', ( #9938 ), #18993, .T. ) ;
#21916 = DIRECTION ( 'NONE',  ( -1.000000000000000000, -5.598259082250514647E-17, -3.330669073875432643E-16 ) ) ;
#21917 = LINE ( 'NONE', #18044, #16795 ) ;
#21918 = CARTESIAN_POINT ( 'NONE',  ( 8.496394830447160373, -0.03251735406450768917, 6.998792816380077220 ) ) ;
#21919 = VERTEX_POINT ( 'NONE', #15447 ) ;
#21921 = ORIENTED_EDGE ( 'NONE', *, *, #18898, .T. ) ;
#21920 = EDGE_LOOP ( 'NONE', ( #17654, #7912, #8698, #8634 ) ) ;
#21922 = EDGE_CURVE ( 'NONE', #10566, #522, #2992, .T. ) ;
#21923 = ORIENTED_EDGE ( 'NONE', *, *, #16750, .T. ) ;
#21924 = ORIENTED_EDGE ( 'NONE', *, *, #19638, .F. ) ;
#21925 = VECTOR ( 'NONE', #4451, 1000.000000000000227 ) ;
#21928 = VERTEX_POINT ( 'NONE', #5227 ) ;
#21927 = EDGE_CURVE ( 'NONE', #10218, #14225, #3280, .T. ) ;
#21926 = ORIENTED_EDGE ( 'NONE', *, *, #9090, .F. ) ;
#21929 = AXIS2_PLACEMENT_3D ( 'NONE', #18182, #2051, #19587 ) ;
#21930 = ORIENTED_EDGE ( 'NONE', *, *, #1687, .T. ) ;
#21931 = VECTOR ( 'NONE', #18230, 1000.000000000000000 ) ;
#21932 = LINE ( 'NONE', #18623, #1621 ) ;
#21933 = CONICAL_SURFACE ( 'NONE', #6510, 5.000000000000000888, 0.7853981633974430610 ) ;
#21934 = EDGE_CURVE ( 'NONE', #15365, #7853, #2132, .T. ) ;
#21935 = ORIENTED_EDGE ( 'NONE', *, *, #8723, .T. ) ;
#21936 = AXIS2_PLACEMENT_3D ( 'NONE', #16546, #5872, #9507 ) ;
#21937 = ORIENTED_EDGE ( 'NONE', *, *, #1912, .T. ) ;
#21938 = VECTOR ( 'NONE', #8612, 1000.000000000000000 ) ;
#21939 = CARTESIAN_POINT ( 'NONE',  ( 4.000000000000003553, 0.000000000000000000, 0.000000000000000000 ) ) ;
#21940 = CARTESIAN_POINT ( 'NONE',  ( -6.000000000000074607, 7.999999999999958256, 7.500000000000062172 ) ) ;
#21941 = LINE ( 'NONE', #20167, #10517 ) ;
#21942 = CARTESIAN_POINT ( 'NONE',  ( -7.710998176012503258, -2.456120859166647019, 8.114728912742579681 ) ) ;
#21943 = FACE_OUTER_BOUND ( 'NONE', #14404, .T. ) ;
#21944 = DIRECTION ( 'NONE',  ( -1.000000000000000000, 4.780126911580487002E-14, -3.854941057726199147E-16 ) ) ;
#21945 = CARTESIAN_POINT ( 'NONE',  ( -6.999999999708142795, 13.99999999900385106, -26.00000000000000000 ) ) ;
#21946 = DIRECTION ( 'NONE',  ( 0.000000000000000000, 3.469446951953619316E-15, 1.000000000000000000 ) ) ;
#21947 = CARTESIAN_POINT ( 'NONE',  ( 30.00000000029184832, 2.999999999003851503, -36.45000000000000284 ) ) ;
#21948 = AXIS2_PLACEMENT_3D ( 'NONE', #23014, #10762, #10421 ) ;
#21949 = CIRCLE ( 'NONE', #20063, 1.500000000000000000 ) ;
#21950 = CARTESIAN_POINT ( 'NONE',  ( 37.35148779274898345, 10.63811079452488961, -2.648512207251442874 ) ) ;
#21951 = CIRCLE ( 'NONE', #17408, 0.5000000000000004441 ) ;
#21952 = VERTEX_POINT ( 'NONE', #1349 ) ;
#21953 = CARTESIAN_POINT ( 'NONE',  ( 36.00000000029184832, 5.999999999003851059, -32.00000000000000000 ) ) ;
#21955 = ORIENTED_EDGE ( 'NONE', *, *, #1882, .F. ) ;
#21954 = VERTEX_POINT ( 'NONE', #14042 ) ;
#21956 = EDGE_CURVE ( 'NONE', #6443, #12862, #21235, .T. ) ;
#21957 = EDGE_LOOP ( 'NONE', ( #1570, #12766 ) ) ;
#21958 = ORIENTED_EDGE ( 'NONE', *, *, #23195, .F. ) ;
#21959 = EDGE_CURVE ( 'NONE', #1433, #21722, #5335, .T. ) ;
#21960 = CYLINDRICAL_SURFACE ( 'NONE', #9165, 0.5000000000000026645 ) ;
#21961 = AXIS2_PLACEMENT_3D ( 'NONE', #19827, #3706, #10876 ) ;
#21962 = AXIS2_PLACEMENT_3D ( 'NONE', #10353, #15528, #15642 ) ;
#21963 = DIRECTION ( 'NONE',  ( 2.775557561562883031E-17, 1.309377075419427801E-16, 1.000000000000000000 ) ) ;
#21964 = CARTESIAN_POINT ( 'NONE',  ( 4.093692494532777282, -4.043567292011544190, 3.733480660068263491E-17 ) ) ;
#21965 = DIRECTION ( 'NONE',  ( 3.330669073875454830E-16, 0.000000000000000000, -1.000000000000000000 ) ) ;
#21966 = DIRECTION ( 'NONE',  ( 0.000000000000000000, 0.000000000000000000, -1.000000000000000000 ) ) ;
#21967 = DIRECTION ( 'NONE',  ( -1.733449886265890494E-32, 7.264582621685753859E-63, 1.000000000000000000 ) ) ;
#21968 = CARTESIAN_POINT ( 'NONE',  ( 2.918498775983380256E-10, 2.999999999003851503, -45.00000000000000000 ) ) ;
#21969 = DIRECTION ( 'NONE',  ( 2.172745813409349776E-17, -1.000000000000000000, 1.309377075419428048E-16 ) ) ;
#21970 = DIRECTION ( 'NONE',  ( -1.000000000000000000, -3.254448077276381206E-32, -1.066788928082016908E-26 ) ) ;
#21971 = EDGE_CURVE ( 'NONE', #5408, #14506, #3453, .T. ) ;
#21972 = CARTESIAN_POINT ( 'NONE',  ( 8.200527591913257197, -1.560621988374212732, 7.318116290495780163 ) ) ;
#21973 = CARTESIAN_POINT ( 'NONE',  ( -5.035458327682192703, 1.561572887838423629, -0.7783303370584467862 ) ) ;
#21974 = CIRCLE ( 'NONE', #20093, 3.500000000000023981 ) ;
#21975 =( NAMED_UNIT ( * ) PLANE_ANGLE_UNIT ( ) SI_UNIT ( $, .RADIAN. ) );
#21976 = CARTESIAN_POINT ( 'NONE',  ( -43.10883117545717624, 4.565685424949221805, 8.000000000000076383 ) ) ;
#21977 = AXIS2_PLACEMENT_3D ( 'NONE', #12601, #14830, #3771 ) ;
#21978 = CARTESIAN_POINT ( 'NONE',  ( 3.972073812946708582, -0.6951863858492013382, -3.565770933504613271 ) ) ;
#21979 = B_SPLINE_CURVE_WITH_KNOTS ( 'NONE', 3,
 ( #11325, #14413, #2282, #188, #9349, #20171 ),
 .UNSPECIFIED., .F., .F.,
 ( 4, 2, 4 ),
 ( 0.002044882221487541018, 0.003063384235218496315, 0.004081886248949452047 ),
 .UNSPECIFIED. ) ;
#21980 = ORIENTED_EDGE ( 'NONE', *, *, #18700, .T. ) ;
#21981 = CARTESIAN_POINT ( 'NONE',  ( 12.84999999999997300, -12.00000000000005151, 2.550000000000038902 ) ) ;
#21982 = DIRECTION ( 'NONE',  ( -0.7313537016191746787, -0.6819983600624941467, -1.072890437865584409E-16 ) ) ;
#21983 = EDGE_LOOP ( 'NONE', ( #16666, #19897, #13095, #7789 ) ) ;
#21984 = CARTESIAN_POINT ( 'NONE',  ( -5.549486778972979373, 36.19267127072042456, -18.86553880985036358 ) ) ;
#21985 = CARTESIAN_POINT ( 'NONE',  ( 24.99999999999995737, 2.000000000000001776, -17.49999999999998224 ) ) ;
#21986 = DIRECTION ( 'NONE',  ( 5.551115123561405253E-17, 1.000000000000000000, -5.963788443470795439E-28 ) ) ;
#21987 = CARTESIAN_POINT ( 'NONE',  ( -89.70000000000064233, 5.551115123125782702E-14, -2.000000000000001776 ) ) ;
#21988 = AXIS2_PLACEMENT_3D ( 'NONE', #20699, #17376, #22458 ) ;
#21989 = VECTOR ( 'NONE', #21761, 1000.000000000000000 ) ;
#21990 = DIRECTION ( 'NONE',  ( 1.000000000000000000, -7.477632011778292156E-48, 3.885780586188017323E-16 ) ) ;
#21991 = CARTESIAN_POINT ( 'NONE',  ( 12.49999999999995914, 2.775557561562891351E-14, -9.500000000000003553 ) ) ;
#21992 = DIRECTION ( 'NONE',  ( -1.000000000000000000, -2.699383410053119644E-30, -3.330669073875432643E-16 ) ) ;
#21993 = DIRECTION ( 'NONE',  ( 0.7313537016191746787, 0.6819983600624940356, 1.072890437865584409E-16 ) ) ;
#21994 = ADVANCED_FACE ( 'NONE', ( #21107 ), #20992, .T. ) ;
#21995 = CARTESIAN_POINT ( 'NONE',  ( 7.499999999999976019, -12.78258024831459139, 9.022398393212654355 ) ) ;
#21996 = CARTESIAN_POINT ( 'NONE',  ( 2.954027403549371644E-15, -3.202582148906737647, -1.452965002680429052 ) ) ;
#21997 = CARTESIAN_POINT ( 'NONE',  ( -53.99613665484950786, 2.700000000000021938, -13.19342998475048212 ) ) ;
#21998 = FACE_OUTER_BOUND ( 'NONE', #277, .T. ) ;
#21999 = CARTESIAN_POINT ( 'NONE',  ( 0.6448876103707898988, 4.246476118072396666, -0.2256878752776944885 ) ) ;
#22000 = FACE_OUTER_BOUND ( 'NONE', #17595, .T. ) ;
#22001 = APPLICATION_PROTOCOL_DEFINITION ( 'draft international standard', 'automotive_design', 1998, #23224 ) ;
#22002 = VERTEX_POINT ( 'NONE', #5102 ) ;
#22003 = APPLICATION_CONTEXT ( 'automotive_design' ) ;
#22005 = VERTEX_POINT ( 'NONE', #22756 ) ;
#22004 = ORIENTED_EDGE ( 'NONE', *, *, #16197, .F. ) ;
#22006 = FACE_OUTER_BOUND ( 'NONE', #6757, .T. ) ;
#22007 = CARTESIAN_POINT ( 'NONE',  ( 37.42127086598689090, 0.2176602893534318184, -2.578729134013127755 ) ) ;
#22008 = ADVANCED_FACE ( 'NONE', ( #3108 ), #1568, .T. ) ;
#22009 = FACE_OUTER_BOUND ( 'NONE', #177, .T. ) ;
#22010 = ORIENTED_EDGE ( 'NONE', *, *, #12002, .F. ) ;
#22011 = DIRECTION ( 'NONE',  ( 2.168404344971004924E-16, 1.000000000000000000, 5.217794476051303021E-47 ) ) ;
#22012 = CYLINDRICAL_SURFACE ( 'NONE', #22563, 0.4999999999999995559 ) ;
#22013 = FACE_OUTER_BOUND ( 'NONE', #13949, .T. ) ;
#22014 = EDGE_CURVE ( 'NONE', #6243, #8200, #12257, .T. ) ;
#22015 = CARTESIAN_POINT ( 'NONE',  ( 0.000000000000000000, -0.5999999999999789946, -3.054668707061614086 ) ) ;
#22016 = FACE_OUTER_BOUND ( 'NONE', #10766, .T. ) ;
#22017 = DIRECTION ( 'NONE',  ( -0.000000000000000000, 1.000000000000000000, 0.000000000000000000 ) ) ;
#22018 = CARTESIAN_POINT ( 'NONE',  ( 0.6554360035617849967, -4.240386000424089197, -5.441324518471480687 ) ) ;
#22019 = EDGE_CURVE ( 'NONE', #273, #1495, #265, .T. ) ;
#22020 = LINE ( 'NONE', #22252, #3303 ) ;
#22021 = EDGE_CURVE ( 'NONE', #10139, #20178, #10508, .T. ) ;
#22022 = LINE ( 'NONE', #11305, #2541 ) ;
#22023 = CARTESIAN_POINT ( 'NONE',  ( 7.573440241539877604, -0.1138337924791416322, 7.421600184846412596 ) ) ;
#22024 = ORIENTED_EDGE ( 'NONE', *, *, #17482, .T. ) ;
#22025 =( GEOMETRIC_REPRESENTATION_CONTEXT ( 3 ) GLOBAL_UNCERTAINTY_ASSIGNED_CONTEXT ( ( #20153 ) ) GLOBAL_UNIT_ASSIGNED_CONTEXT ( ( #1627, #16079, #10682 ) ) REPRESENTATION_CONTEXT ( 'NONE', 'WORKASPACE' ) );
#22026 = SURFACE_STYLE_FILL_AREA ( #12977 ) ;
#22028 = ORIENTED_EDGE ( 'NONE', *, *, #19313, .T. ) ;
#22027 = ORIENTED_EDGE ( 'NONE', *, *, #23171, .T. ) ;
#22029 = UNCERTAINTY_MEASURE_WITH_UNIT (LENGTH_MEASURE( 1.000000000000000082E-05 ), #18484, 'distance_accuracy_value', 'NONE');
#22030 = ORIENTED_EDGE ( 'NONE', *, *, #16826, .T. ) ;
#22031 = ORIENTED_EDGE ( 'NONE', *, *, #17331, .T. ) ;
#22033 = ORIENTED_EDGE ( 'NONE', *, *, #13569, .T. ) ;
#22032 = ORIENTED_EDGE ( 'NONE', *, *, #22468, .T. ) ;
#22034 = ORIENTED_EDGE ( 'NONE', *, *, #18696, .T. ) ;
#22035 = CYLINDRICAL_SURFACE ( 'NONE', #11739, 2.550000000000003819 ) ;
#22036 = EDGE_CURVE ( 'NONE', #8174, #4432, #11514, .T. ) ;
#22037 = ORIENTED_EDGE ( 'NONE', *, *, #2196, .F. ) ;
#22038 =( BOUNDED_SURFACE ( )  B_SPLINE_SURFACE ( 3, 2, ( 
 ( #9613, #7848, #22200 ),
 ( #1960, #10901, #9156 ),
 ( #16316, #221, #7388 ),
 ( #21748, #5630, #11598 ),
 ( #918, #19022, #20905 ),
 ( #13836, #20553, #13609 ),
 ( #10184, #2546, #6205 ),
 ( #13495, #13374, #17116 ) ),
 .UNSPECIFIED., .F., .F., .T. ) 
 B_SPLINE_SURFACE_WITH_KNOTS ( ( 4, 2, 2, 4 ),
 ( 3, 3 ),
 ( 3.665191429188095817, 3.926990816987244504, 4.188790204786393190, 4.712388980384689674 ),
 ( 0.000000000000000000, 1.000000000000000000 ),
 .UNSPECIFIED. ) 
 GEOMETRIC_REPRESENTATION_ITEM ( )  RATIONAL_B_SPLINE_SURFACE ( (
 ( 1.000000000000000000, 0.7905694150421765931, 1.000000000000000000),
 ( 1.000000000000000000, 0.8144940154005562150, 1.000000000000000000),
 ( 1.000000000000000000, 0.8408337562111960484, 1.000000000000000000),
 ( 1.000000000000000000, 0.8912170513578050457, 1.000000000000000000),
 ( 1.000000000000000000, 0.9152160911082583006, 1.000000000000000000),
 ( 1.000000000000000000, 0.9758108578640632969, 1.000000000000000000),
 ( 1.000000000000000000, 1.000509427570040133, 1.000000000000000000),
 ( 1.000000000000000000, 1.000000000000000000, 1.000000000000000000) ) ) 
 REPRESENTATION_ITEM ( '' )  SURFACE ( )  );
#22039 = ORIENTED_EDGE ( 'NONE', *, *, #10792, .T. ) ;
#22040 = ORIENTED_EDGE ( 'NONE', *, *, #10188, .T. ) ;
#22041 = ADVANCED_FACE ( 'NONE', ( #12496 ), #14646, .F. ) ;
#22042 = CARTESIAN_POINT ( 'NONE',  ( 0.000000000000000000, -3.031088913245536087, 1.750000000000003331 ) ) ;
#22043 = EDGE_CURVE ( 'NONE', #10215, #4400, #17448, .T. ) ;
#22044 = CARTESIAN_POINT ( 'NONE',  ( 3.853576393533437815E-15, -0.3420925509381499419, -3.500000000000009770 ) ) ;
#22045 = CARTESIAN_POINT ( 'NONE',  ( 4.207491450040564018, -2.029819825146498502, -3.671670828759570959 ) ) ;
#22046 = DIRECTION ( 'NONE',  ( -0.6819983600625060260, -0.7313537016191634654, 0.000000000000000000 ) ) ;
#22047 = CARTESIAN_POINT ( 'NONE',  ( -95.70000000000058549, -0.5000000000000975886, 1.000000000000014655 ) ) ;
#22048 = AXIS2_PLACEMENT_3D ( 'NONE', #6523, #13350, #9705 ) ;
#22049 = CARTESIAN_POINT ( 'NONE',  ( 4.071447262713891568, -2.020725942163709377, -3.499999999999999556 ) ) ;
#22050 = CARTESIAN_POINT ( 'NONE',  ( 1.387778780781445676E-14, -22.49999999999995737, -2.775557561562891351E-14 ) ) ;
#22051 = DIRECTION ( 'NONE',  ( 0.000000000000000000, -1.000000000000000000, 0.000000000000000000 ) ) ;
#22052 = CIRCLE ( 'NONE', #10775, 6.249999999999992006 ) ;
#22053 = ADVANCED_FACE ( 'NONE', ( #20147 ), #3563, .T. ) ;
#22054 = CARTESIAN_POINT ( 'NONE',  ( -64.00000000000045475, 6.245004513516505540E-14, -1.999999999999974021 ) ) ;
#22055 = PLANE ( 'NONE',  #2534 ) ;
#22056 = EDGE_CURVE ( 'NONE', #5230, #7393, #22151, .T. ) ;
#22057 = CARTESIAN_POINT ( 'NONE',  ( 7.000000000000006217, -2.645898033750298417, 9.250000000000021316 ) ) ;
#22058 = ORIENTED_EDGE ( 'NONE', *, *, #11092, .F. ) ;
#22059 = PRODUCT_DEFINITION_CONTEXT ( 'detailed design', #19916, 'design' ) ;
#22060 = SHAPE_REPRESENTATION_RELATIONSHIP ( 'NONE' , 'NONE' ,  #4439, #11971 ) ;
#22061 = FACE_OUTER_BOUND ( 'NONE', #3526, .T. ) ;
#22063 = EDGE_LOOP ( 'NONE', ( #13925, #9618, #5693, #3884 ) ) ;
#22062 = EDGE_LOOP ( 'NONE', ( #7454, #4866, #899, #8551 ) ) ;
#22064 = CIRCLE ( 'NONE', #14533, 2.000000000000015543 ) ;
#22065 = ORIENTED_EDGE ( 'NONE', *, *, #18864, .F. ) ;
#22066 = CIRCLE ( 'NONE', #19816, 2.549999999999996714 ) ;
#22067 = EDGE_LOOP ( 'NONE', ( #13705, #22065, #23118, #4431 ) ) ;
#22068 = ORIENTED_EDGE ( 'NONE', *, *, #19004, .T. ) ;
#22069 = DIRECTION ( 'NONE',  ( -1.000000000000000000, 1.696174065399527605E-14, -3.854941057726199147E-16 ) ) ;
#22070 = VECTOR ( 'NONE', #15267, 1000.000000000000000 ) ;
#22071 = DIRECTION ( 'NONE',  ( -1.000000000000000000, 2.168404344971005170E-16, -1.203141491611682442E-30 ) ) ;
#22072 = EDGE_LOOP ( 'NONE', ( #22010, #13183, #5850, #17934 ) ) ;
#22073 = DIRECTION ( 'NONE',  ( -0.7071067811865534569, -0.7071067811865416886, -1.565905175853764455E-16 ) ) ;
#22074 = DIRECTION ( 'NONE',  ( -1.000000000000000000, 0.000000000000000000, 0.000000000000000000 ) ) ;
#22075 = CARTESIAN_POINT ( 'NONE',  ( 77.42435809754130105, -10.99999999999981526, 6.000000000000123457 ) ) ;
#22076 = CIRCLE ( 'NONE', #20570, 0.4999999999999978351 ) ;
#22077 = FACE_OUTER_BOUND ( 'NONE', #7154, .T. ) ;
#22078 = ADVANCED_FACE ( 'NONE', ( #7222 ), #19922, .T. ) ;
#22079 = CARTESIAN_POINT ( 'NONE',  ( -8.037202331403117128, -11.80340871766187405, 7.528743044528739325 ) ) ;
#22080 = AXIS2_PLACEMENT_3D ( 'NONE', #17710, #10427, #9014 ) ;
#22081 = CARTESIAN_POINT ( 'NONE',  ( -7.576750937466491642, -2.112750738699229469, 7.200086239787990117 ) ) ;
#22082 = CARTESIAN_POINT ( 'NONE',  ( 4.690415759823387987, -0.7499999999999520384, -3.000000000000002665 ) ) ;
#22083 = FACE_OUTER_BOUND ( 'NONE', #2495, .T. ) ;
#22084 = VECTOR ( 'NONE', #4444, 1000.000000000000114 ) ;
#22085 = FACE_BOUND ( 'NONE', #21505, .T. ) ;
#22086 = EDGE_CURVE ( 'NONE', #5438, #22523, #22064, .T. ) ;
#22087 = AXIS2_PLACEMENT_3D ( 'NONE', #12285, #21490, #14069 ) ;
#22088 = TOROIDAL_SURFACE ( 'NONE', #19076, 6.700000000000001066, 0.5000000000000000000 ) ;
#22089 = DIRECTION ( 'NONE',  ( 1.000000000000000000, 1.110223024625164429E-16, -1.298062744027674633E-32 ) ) ;
#22090 = CARTESIAN_POINT ( 'NONE',  ( 4.180232103119976728, 2.085387772176682919, -3.570466442734708590 ) ) ;
#22091 = ORIENTED_EDGE ( 'NONE', *, *, #8834, .F. ) ;
#22092 = ORIENTED_EDGE ( 'NONE', *, *, #2034, .F. ) ;
#22093 = AXIS2_PLACEMENT_3D ( 'NONE', #9703, #6057, #13226 ) ;
#22094 = CARTESIAN_POINT ( 'NONE',  ( 36.00000000029184832, -9.961476088449217059E-10, -18.50000000000000355 ) ) ;
#22095 = DIRECTION ( 'NONE',  ( 0.6819983600624951459, 0.7313537016191735685, 7.771699578536686021E-16 ) ) ;
#22096 = VERTEX_POINT ( 'NONE', #14386 ) ;
#22097 = AXIS2_PLACEMENT_3D ( 'NONE', #18807, #2680, #11617 ) ;
#22098 = CYLINDRICAL_SURFACE ( 'NONE', #852, 6.000000000000037303 ) ;
#22099 = CARTESIAN_POINT ( 'NONE',  ( 12.84999999999997300, -1.999999999999998224, 2.549999999999997158 ) ) ;
#22100 = CARTESIAN_POINT ( 'NONE',  ( -50.65685424949277404, -0.5000000000001045830, -7.500000000000062172 ) ) ;
#22101 = CARTESIAN_POINT ( 'NONE',  ( 2.742413778650823364, -1.325747111984059590, -4.750000000000000888 ) ) ;
#22102 = CIRCLE ( 'NONE', #1428, 0.5000000000000029976 ) ;
#22103 = LINE ( 'NONE', #2099, #22295 ) ;
#22104 = TOROIDAL_SURFACE ( 'NONE', #11948, 4.500000000000000888, 0.5000000000000000000 ) ;
#22105 = CARTESIAN_POINT ( 'NONE',  ( 5.599999999999994316, -4.041451884327383226, 0.000000000000000000 ) ) ;
#22106 = LINE ( 'NONE', #6344, #14691 ) ;
#22107 = ADVANCED_FACE ( 'NONE', ( #19803 ), #21806, .F. ) ;
#22108 = DIRECTION ( 'NONE',  ( 3.241725282392603095E-30, 1.000000000000000000, -2.218671295934100958E-31 ) ) ;
#22109 = CARTESIAN_POINT ( 'NONE',  ( 7.951003271401684280, -13.83829779185628794, 7.659883344695716190 ) ) ;
#22110 = CARTESIAN_POINT ( 'NONE',  ( 0.000000000000000000, 0.000000000000000000, 0.000000000000000000 ) ) ;
#22111 = CYLINDRICAL_SURFACE ( 'NONE', #1256, 3.000000000000011102 ) ;
#22112 = DIRECTION ( 'NONE',  ( -1.733449886265891589E-32, 4.190823558986610327E-31, -1.000000000000000000 ) ) ;
#22113 = PRESENTATION_STYLE_ASSIGNMENT (( #20241 ) ) ;
#22114 = EDGE_CURVE ( 'NONE', #11691, #20589, #16937, .T. ) ;
#22115 = AXIS2_PLACEMENT_3D ( 'NONE', #4943, #2963, #5306 ) ;
#22116 = CARTESIAN_POINT ( 'NONE',  ( 0.3126073911696447549, 2.020725942163625888, -3.499999999999996003 ) ) ;
#22117 = AXIS2_PLACEMENT_3D ( 'NONE', #3514, #14328, #19751 ) ;
#22118 = CONICAL_SURFACE ( 'NONE', #10101, 4.750000000000013323, 0.6593100683328582123 ) ;
#22119 = EDGE_LOOP ( 'NONE', ( #1015, #6886, #3023, #8244 ) ) ;
#22120 = EDGE_CURVE ( 'NONE', #8376, #7460, #21169, .T. ) ;
#22122 = ORIENTED_EDGE ( 'NONE', *, *, #18366, .T. ) ;
#22121 = EDGE_LOOP ( 'NONE', ( #6152, #5494 ) ) ;
#22123 = CARTESIAN_POINT ( 'NONE',  ( -6.000000000000074607, 7.499999999999958256, 7.500000000000062172 ) ) ;
#22124 = CARTESIAN_POINT ( 'NONE',  ( 3.999999999999955147, -2.309401076758532678, -3.433295621305388678 ) ) ;
#22125 = ORIENTED_EDGE ( 'NONE', *, *, #9147, .F. ) ;
#22126 = CARTESIAN_POINT ( 'NONE',  ( 4.104070371397483541, 4.047367226856696476, 6.938893903907228378E-15 ) ) ;
#22127 = FACE_OUTER_BOUND ( 'NONE', #3997, .T. ) ;
#22128 = FACE_OUTER_BOUND ( 'NONE', #16770, .T. ) ;
#22129 = CARTESIAN_POINT ( 'NONE',  ( -50.65685424949281668, 2.700000000000021938, -7.500000000000089706 ) ) ;
#22130 = LINE ( 'NONE', #20260, #12166 ) ;
#22131 = AXIS2_PLACEMENT_3D ( 'NONE', #12639, #21378, #1481 ) ;
#22132 = DIRECTION ( 'NONE',  ( 2.168404344971004924E-16, 1.000000000000000000, 5.217794476051303021E-47 ) ) ;
#22133 = CARTESIAN_POINT ( 'NONE',  ( -1.387778780781445676E-14, 2.000000000000001776, -2.000000000000001776 ) ) ;
#22134 = DIRECTION ( 'NONE',  ( 0.000000000000000000, 0.000000000000000000, 1.000000000000000000 ) ) ;
#22135 = DIRECTION ( 'NONE',  ( 0.000000000000000000, 0.000000000000000000, 1.000000000000000000 ) ) ;
#22136 = CARTESIAN_POINT ( 'NONE',  ( 4.330127018922103055, 4.999999999999838352, 7.499999999999971578 ) ) ;
#22137 = VECTOR ( 'NONE', #11759, 1000.000000000000000 ) ;
#22138 = CARTESIAN_POINT ( 'NONE',  ( 118.6341267379645501, -2.990348597579822965, 6.500000000000130562 ) ) ;
#22139 = DIRECTION ( 'NONE',  ( -9.121204216617949000E-31, -1.000000000000000000, 6.982962677686261977E-15 ) ) ;
#22140 = COLOUR_RGB ( '', 0.08235294, 0.09019608, 0.10196078) ;
#22141 = EDGE_LOOP ( 'NONE', ( #87, #10663, #10969, #6634 ) ) ;
#22142 = EDGE_CURVE ( 'NONE', #1547, #11088, #9281, .T. ) ;
#22143 =( NAMED_UNIT ( * ) PLANE_ANGLE_UNIT ( ) SI_UNIT ( $, .RADIAN. ) );
#22145 = ORIENTED_EDGE ( 'NONE', *, *, #8507, .F. ) ;
#22144 = ORIENTED_EDGE ( 'NONE', *, *, #16535, .T. ) ;
#22146 = EDGE_CURVE ( 'NONE', #6727, #280, #22430, .T. ) ;
#22147 = ORIENTED_EDGE ( 'NONE', *, *, #19725, .T. ) ;
#22148 = ORIENTED_EDGE ( 'NONE', *, *, #9269, .T. ) ;
#22150 = ORIENTED_EDGE ( 'NONE', *, *, #21049, .T. ) ;
#22149 = VERTEX_POINT ( 'NONE', #2607 ) ;
#22151 = B_SPLINE_CURVE_WITH_KNOTS ( 'NONE', 3,
 ( #3790, #7450, #5811, #54 ),
 .UNSPECIFIED., .F., .F.,
 ( 4, 4 ),
 ( 2.380739282183830354E-07, 0.002044882221487538416 ),
 .UNSPECIFIED. ) ;
#22152 = ORIENTED_EDGE ( 'NONE', *, *, #16395, .T. ) ;
#22153 = DIRECTION ( 'NONE',  ( 0.000000000000000000, 1.000000000000000000, 0.000000000000000000 ) ) ;
#22154 = ORIENTED_EDGE ( 'NONE', *, *, #10387, .T. ) ;
#22155 = ORIENTED_EDGE ( 'NONE', *, *, #17939, .T. ) ;
#22156 = VERTEX_POINT ( 'NONE', #22381 ) ;
#22157 = CARTESIAN_POINT ( 'NONE',  ( -4.499999999708154341, 35.49999999900384751, -22.50000000000000000 ) ) ;
#22158 = ADVANCED_FACE ( 'NONE', ( #22255 ), #851, .T. ) ;
#22159 = AXIS2_PLACEMENT_3D ( 'NONE', #1470, #8645, #15802 ) ;
#22160 = DIRECTION ( 'NONE',  ( -3.330669073875432643E-16, -4.437342591868153746E-31, 1.000000000000000000 ) ) ;
#22161 = CARTESIAN_POINT ( 'NONE',  ( 6.000000000291855429, 2.999999999003851503, -41.55000000000000426 ) ) ;
#22162 = DIRECTION ( 'NONE',  ( -3.070652698126927723E-17, -1.000000000000000000, 4.167305704548413124E-17 ) ) ;
#22163 = EDGE_CURVE ( 'NONE', #5689, #8200, #6263, .T. ) ;
#22164 =( GEOMETRIC_REPRESENTATION_CONTEXT ( 3 ) GLOBAL_UNCERTAINTY_ASSIGNED_CONTEXT ( ( #5844 ) ) GLOBAL_UNIT_ASSIGNED_CONTEXT ( ( #18615, #18727, #741 ) ) REPRESENTATION_CONTEXT ( 'NONE', 'WORKASPACE' ) );
#22165 = DIRECTION ( 'NONE',  ( -5.551115123561405253E-17, -1.000000000000000000, -2.256980353643891447E-27 ) ) ;
#22166 = DIRECTION ( 'NONE',  ( -2.013525853228507892E-32, -6.902532920683810383E-31, 1.000000000000000000 ) ) ;
#22167 = LINE ( 'NONE', #10984, #17220 ) ;
#22168 = CARTESIAN_POINT ( 'NONE',  ( -3.122502256758252770E-14, 59.74999999999991473, 2.081668171172168513E-14 ) ) ;
#22169 = DIRECTION ( 'NONE',  ( 7.027852765209223361E-16, 0.5000000000000009992, -0.8660254037844381525 ) ) ;
#22170 = CARTESIAN_POINT ( 'NONE',  ( 0.03027795055835478741, 0.6888063905328364323, -3.500000000000034639 ) ) ;
#22171 = FACE_BOUND ( 'NONE', #8038, .T. ) ;
#22172 = CARTESIAN_POINT ( 'NONE',  ( 108.2426266706970637, -10.52760560296347947, 6.500000000000019540 ) ) ;
#22173 = ORIENTED_EDGE ( 'NONE', *, *, #3827, .T. ) ;
#22174 = EDGE_CURVE ( 'NONE', #278, #6998, #15418, .T. ) ;
#22175 = EDGE_CURVE ( 'NONE', #15911, #20996, #10038, .T. ) ;
#22176 = CIRCLE ( 'NONE', #19914, 2.550000000000012701 ) ;
#22178 = ORIENTED_EDGE ( 'NONE', *, *, #8083, .F. ) ;
#22177 = ORIENTED_EDGE ( 'NONE', *, *, #9946, .T. ) ;
#22179 =( REPRESENTATION_RELATIONSHIP ('NONE','NONE', #19450, #17992 ) REPRESENTATION_RELATIONSHIP_WITH_TRANSFORMATION ( #18941 )SHAPE_REPRESENTATION_RELATIONSHIP( ) );
#22180 = EDGE_CURVE ( 'NONE', #12208, #10144, #15303, .T. ) ;
#22181 = ORIENTED_EDGE ( 'NONE', *, *, #21858, .T. ) ;
#22182 = ORIENTED_EDGE ( 'NONE', *, *, #14589, .F. ) ;
#22183 = ORIENTED_EDGE ( 'NONE', *, *, #8263, .T. ) ;
#22184 = DIRECTION ( 'NONE',  ( 2.013525853228507892E-32, 6.902532920683810383E-31, -1.000000000000000000 ) ) ;
#22185 = EDGE_CURVE ( 'NONE', #11088, #1547, #4378, .T. ) ;
#22186 = EDGE_CURVE ( 'NONE', #3456, #21586, #17933, .T. ) ;
#22187 = DIRECTION ( 'NONE',  ( -0.7313537016191756779, 0.6819983600624930364, -4.000536147326505450E-15 ) ) ;
#22188 = ORIENTED_EDGE ( 'NONE', *, *, #15859, .F. ) ;
#22189 = DIRECTION ( 'NONE',  ( -2.710505431213791653E-16, -1.000000000000000000, 4.807121141190541565E-31 ) ) ;
#22190 = CARTESIAN_POINT ( 'NONE',  ( 24.99999999999998579, 1.249999999999987121, -17.00000000000001066 ) ) ;
#22191 = DIRECTION ( 'NONE',  ( 0.7313537016191745677, 0.6819983600624940356, 1.072890437865584285E-16 ) ) ;
#22192 = AXIS2_PLACEMENT_3D ( 'NONE', #19676, #12016, #17432 ) ;
#22193 = CARTESIAN_POINT ( 'NONE',  ( 6.000000000291855429, -9.961476088449217059E-10, -45.00000000000000000 ) ) ;
#22194 = CARTESIAN_POINT ( 'NONE',  ( -7.263517083688649123, -11.72058614530575049, 7.724990489865638743 ) ) ;
#22195 = CARTESIAN_POINT ( 'NONE',  ( -3.499999999708153453, 35.49999999900384751, -25.50000000000000000 ) ) ;
#22196 = CARTESIAN_POINT ( 'NONE',  ( -2.428612866367529932E-14, 60.00000000000000000, 6.938893903907228378E-15 ) ) ;
#22197 = EDGE_CURVE ( 'NONE', #21644, #5438, #8156, .T. ) ;
#22198 = CARTESIAN_POINT ( 'NONE',  ( 4.000000000000003553, 2.309401076758480720, -5.600000000000000533 ) ) ;
#22199 = EDGE_CURVE ( 'NONE', #19105, #22821, #1030, .T. ) ;
#22200 = CARTESIAN_POINT ( 'NONE',  ( 37.00000000000030553, 0.2500000000000148215, -10.43301270189226138 ) ) ;
#22201 = EDGE_CURVE ( 'NONE', #13412, #5493, #14914, .T. ) ;
#22202 = EDGE_CURVE ( 'NONE', #7853, #9785, #9646, .T. ) ;
#22203 =( LENGTH_UNIT ( ) NAMED_UNIT ( * ) SI_UNIT ( .MILLI., .METRE. ) );
#22204 = DIRECTION ( 'NONE',  ( 0.7071067811865490160, 0.7071067811865460184, 1.565905175853767167E-16 ) ) ;
#22205 = CARTESIAN_POINT ( 'NONE',  ( 0.2182387239012628377, 1.693823289460905768, 3.499999999999994227 ) ) ;
#22206 = ORIENTED_EDGE ( 'NONE', *, *, #2789, .T. ) ;
#22207 = ORIENTED_EDGE ( 'NONE', *, *, #17411, .F. ) ;
#22208 = VECTOR ( 'NONE', #15984, 1000.000000000000000 ) ;
#22209 = ORIENTED_EDGE ( 'NONE', *, *, #1878, .F. ) ;
#22211 = ORIENTED_EDGE ( 'NONE', *, *, #5015, .F. ) ;
#22210 = EDGE_CURVE ( 'NONE', #9224, #18765, #11655, .T. ) ;
#22212 = ORIENTED_EDGE ( 'NONE', *, *, #22898, .F. ) ;
#22213 = DIRECTION ( 'NONE',  ( 2.859620781426167795E-30, 1.000000000000000000, -7.806255641895663479E-15 ) ) ;
#22214 = CYLINDRICAL_SURFACE ( 'NONE', #9089, 0.2500000000000003331 ) ;
#22215 = VERTEX_POINT ( 'NONE', #18490 ) ;
#22216 = EDGE_CURVE ( 'NONE', #5349, #22506, #17061, .T. ) ;
#22217 = CARTESIAN_POINT ( 'NONE',  ( -3.999999999708153453, 35.99999999900384751, -18.50000000000000355 ) ) ;
#22218 = CARTESIAN_POINT ( 'NONE',  ( 4.175813232069142344, -2.061359961916364725, 3.570380186727402538 ) ) ;
#22219 = CARTESIAN_POINT ( 'NONE',  ( -45.01801948466091829, 6.474873734152897242, 7.500000000000034639 ) ) ;
#22220 = DIRECTION ( 'NONE',  ( 0.000000000000000000, 3.382522293539642133E-32, 1.000000000000000000 ) ) ;
#22221 = B_SPLINE_CURVE_WITH_KNOTS ( 'NONE', 3,
 ( #18773, #20543, #4646, #22536, #1012 ),
 .UNSPECIFIED., .F., .F.,
 ( 4, 1, 4 ),
 ( 0.000000000000000000, 0.002020725942163691374, 0.004041451884327382747 ),
 .UNSPECIFIED. ) ;
#22222 = CYLINDRICAL_SURFACE ( 'NONE', #16558, 10.00000000000006395 ) ;
#22223 = DIRECTION ( 'NONE',  ( -1.000000000000000000, 1.550910762415526064E-16, 0.000000000000000000 ) ) ;
#22224 = DIRECTION ( 'NONE',  ( 0.1556420233463076119, 0.000000000000000000, 0.9878135252003121813 ) ) ;
#22225 = DIRECTION ( 'NONE',  ( 1.000000000000000000, -1.276756478318923119E-15, 1.239088197126283964E-15 ) ) ;
#22226 = AXIS2_PLACEMENT_3D ( 'NONE', #2681, #18808, #8101 ) ;
#22227 = VECTOR ( 'NONE', #3738, 1000.000000000000000 ) ;
#22228 = CARTESIAN_POINT ( 'NONE',  ( 4.086262629614032527, 4.082406995609999534, 0.07093633357109276061 ) ) ;
#22229 = CARTESIAN_POINT ( 'NONE',  ( 4.071447262713884463, 2.020725942163688504, -3.499999999999999556 ) ) ;
#22230 = DIRECTION ( 'NONE',  ( 0.000000000000000000, 0.000000000000000000, -1.000000000000000000 ) ) ;
#22231 = CARTESIAN_POINT ( 'NONE',  ( 4.082498951862916670, 2.020725942163687616, -3.500000000000001332 ) ) ;
#22232 = ORIENTED_EDGE ( 'NONE', *, *, #6698, .T. ) ;
#22233 = ORIENTED_EDGE ( 'NONE', *, *, #18416, .F. ) ;
#22235 = ORIENTED_EDGE ( 'NONE', *, *, #16818, .T. ) ;
#22234 = EDGE_LOOP ( 'NONE', ( #5517, #631, #15771, #13232 ) ) ;
#22236 = AXIS2_PLACEMENT_3D ( 'NONE', #13369, #5970, #11592 ) ;
#22237 = CIRCLE ( 'NONE', #12059, 0.5000000000000004441 ) ;
#22238 = LINE ( 'NONE', #16693, #17800 ) ;
#22239 = ADVANCED_FACE ( 'NONE', ( #2374 ), #2897, .T. ) ;
#22240 = CARTESIAN_POINT ( 'NONE',  ( 2.298974087852386550, -1.453757124409941204, -4.750000000000024869 ) ) ;
#22241 = DIRECTION ( 'NONE',  ( 1.066786462891689527E-26, 6.656013887802287108E-31, 1.000000000000000000 ) ) ;
#22242 = VERTEX_POINT ( 'NONE', #7787 ) ;
#22243 = CARTESIAN_POINT ( 'NONE',  ( 7.949747468597695210, 47.94974746730969173, -19.49999999999998934 ) ) ;
#22244 = CARTESIAN_POINT ( 'NONE',  ( 119.5756419024615411, -7.000000000000006217, 6.500000000000103029 ) ) ;
#22245 = CARTESIAN_POINT ( 'NONE',  ( 4.124214193018073793, -2.028338413290942110, 3.513185186763553958 ) ) ;
#22246 = CARTESIAN_POINT ( 'NONE',  ( -6.056833031243687770, 36.14537244600960975, -16.80371197567150432 ) ) ;
#22247 = PRESENTATION_STYLE_ASSIGNMENT (( #7668 ) ) ;
#22248 = AXIS2_PLACEMENT_3D ( 'NONE', #5684, #10733, #14614 ) ;
#22249 = CARTESIAN_POINT ( 'NONE',  ( 2.775557561562891351E-14, 5.500000000000001776, -6.499999999999950262 ) ) ;
#22250 = CARTESIAN_POINT ( 'NONE',  ( -1.660531772554314722, 3.660093687634845772, 3.346627174601739456E-15 ) ) ;
#22251 = CARTESIAN_POINT ( 'NONE',  ( -4.550510256924974684, 35.99999999900384751, -19.50000000000000355 ) ) ;
#22252 = CARTESIAN_POINT ( 'NONE',  ( 42.00000000000014921, 0.000000000000000000, -6.499999999999950262 ) ) ;
#22253 = AXIS2_PLACEMENT_3D ( 'NONE', #3394, #22800, #6795 ) ;
#22254 = CARTESIAN_POINT ( 'NONE',  ( 3.973110223768741456, 0.6864646529411790876, 3.565797985667471970 ) ) ;
#22256 = AXIS2_PLACEMENT_3D ( 'NONE', #6336, #810, #13741 ) ;
#22255 = FACE_OUTER_BOUND ( 'NONE', #5666, .T. ) ;
#22257 = AXIS2_PLACEMENT_3D ( 'NONE', #4654, #8428, #13486 ) ;
#22258 = VERTEX_POINT ( 'NONE', #18613 ) ;
#22260 = ORIENTED_EDGE ( 'NONE', *, *, #2623, .F. ) ;
#22259 = ORIENTED_EDGE ( 'NONE', *, *, #4332, .T. ) ;
#22261 = UNCERTAINTY_MEASURE_WITH_UNIT (LENGTH_MEASURE( 1.000000000000000082E-05 ), #4666, 'distance_accuracy_value', 'NONE');
#22262 = VERTEX_POINT ( 'NONE', #16825 ) ;
#22263 = EDGE_LOOP ( 'NONE', ( #13265, #3804, #2910, #10515 ) ) ;
#22265 = ORIENTED_EDGE ( 'NONE', *, *, #2965, .T. ) ;
#22264 = ORIENTED_EDGE ( 'NONE', *, *, #14555, .F. ) ;
#22266 = B_SPLINE_CURVE_WITH_KNOTS ( 'NONE', 3,
 ( #20262, #3780, #23135, #18258, #3373, #7775 ),
 .UNSPECIFIED., .F., .F.,
 ( 4, 2, 4 ),
 ( 0.006456566858647415710, 0.007625406818786682923, 0.008794246778925950137 ),
 .UNSPECIFIED. ) ;
#22267 = CARTESIAN_POINT ( 'NONE',  ( -5.035458327682264645, -1.561572887838380108, 0.7783303370584921943 ) ) ;
#22268 = DIRECTION ( 'NONE',  ( 0.000000000000000000, 0.000000000000000000, 1.000000000000000000 ) ) ;
#22269 = VERTEX_POINT ( 'NONE', #12440 ) ;
#22270 = CARTESIAN_POINT ( 'NONE',  ( 2.775557561562891351E-14, 1.387778780781445676E-14, -9.999999999999968026 ) ) ;
#22271 = VECTOR ( 'NONE', #16501, 1000.000000000000000 ) ;
#22272 = CARTESIAN_POINT ( 'NONE',  ( 3.999999999999948042, 2.309401076758532678, -3.433295621305378020 ) ) ;
#22273 = FACE_OUTER_BOUND ( 'NONE', #8176, .T. ) ;
#22274 = AXIS2_PLACEMENT_3D ( 'NONE', #21479, #17577, #8761 ) ;
#22275 = CARTESIAN_POINT ( 'NONE',  ( -90.63385214007838897, -0.5000000000000628386, -7.926881151201908615 ) ) ;
#22276 = AXIS2_PLACEMENT_3D ( 'NONE', #11100, #21710, #2399 ) ;
#22277 = CARTESIAN_POINT ( 'NONE',  ( -6.999999999708142795, 35.99999999900384751, -19.00000000000000355 ) ) ;
#22278 = AXIS2_PLACEMENT_3D ( 'NONE', #7461, #3271, #10547 ) ;
#22279 = DIRECTION ( 'NONE',  ( 0.000000000000000000, -6.938893903907238633E-15, -1.000000000000000000 ) ) ;
#22280 = CARTESIAN_POINT ( 'NONE',  ( 7.024848138040876044, -2.659619850263452268, 8.468562630484324671 ) ) ;
#22281 = CARTESIAN_POINT ( 'NONE',  ( -55.05572809000123868, -0.5000000000001045830, -7.500000000000062172 ) ) ;
#22282 = DIRECTION ( 'NONE',  ( -1.000000000000000000, -4.440892098500626162E-16, 5.551115123125782702E-16 ) ) ;
#22283 = EDGE_CURVE ( 'NONE', #927, #17692, #14812, .T. ) ;
#22284 = CARTESIAN_POINT ( 'NONE',  ( 4.750000000000028422, 3.258504577274833815E-14, -3.000000000000002665 ) ) ;
#22285 = FACE_OUTER_BOUND ( 'NONE', #19423, .T. ) ;
#22286 = LINE ( 'NONE', #4746, #20218 ) ;
#22287 = LINE ( 'NONE', #1001, #13782 ) ;
#22288 = EDGE_LOOP ( 'NONE', ( #23238, #9443 ) ) ;
#22289 = UNCERTAINTY_MEASURE_WITH_UNIT (LENGTH_MEASURE( 1.000000000000000082E-05 ), #17812, 'distance_accuracy_value', 'NONE');
#22290 = AXIS2_PLACEMENT_3D ( 'NONE', #16911, #17864, #23167 ) ;
#22291 =( LENGTH_UNIT ( ) NAMED_UNIT ( * ) SI_UNIT ( .MILLI., .METRE. ) );
#22292 = CIRCLE ( 'NONE', #20414, 4.750000000000013323 ) ;
#22294 = VERTEX_POINT ( 'NONE', #1740 ) ;
#22293 = EDGE_LOOP ( 'NONE', ( #9427, #13264, #3019, #14135 ) ) ;
#22295 = VECTOR ( 'NONE', #237, 1000.000000000000000 ) ;
#22296 = CIRCLE ( 'NONE', #22671, 0.5000000000000004441 ) ;
#22297 = AXIS2_PLACEMENT_3D ( 'NONE', #375, #3885, #2004 ) ;
#22298 = VERTEX_POINT ( 'NONE', #19752 ) ;
#22299 = AXIS2_PLACEMENT_3D ( 'NONE', #20358, #7888, #18707 ) ;
#22300 = EDGE_LOOP ( 'NONE', ( #2518, #21287, #10717, #6839 ) ) ;
#22301 = ADVANCED_FACE ( 'NONE', ( #3405 ), #10787, .T. ) ;
#22302 = EDGE_LOOP ( 'NONE', ( #5589, #15097, #11856, #16947 ) ) ;
#22303 = ORIENTED_EDGE ( 'NONE', *, *, #4262, .T. ) ;
#22304 = CARTESIAN_POINT ( 'NONE',  ( 3.000000000291852764, 42.99999999900385461, -15.99999999999999289 ) ) ;
#22305 = DIRECTION ( 'NONE',  ( -1.000000000000000000, 0.000000000000000000, 0.000000000000000000 ) ) ;
#22306 = ORIENTED_EDGE ( 'NONE', *, *, #108, .T. ) ;
#22307 = CARTESIAN_POINT ( 'NONE',  ( 4.082498951862917558, -4.041451884327432076, 1.040834085586084257E-14 ) ) ;
#22308 = ADVANCED_FACE ( 'NONE', ( #3632, #17988 ), #21412, .F. ) ;
#22309 = TOROIDAL_SURFACE ( 'NONE', #15161, 6.500000000000000888, 0.5000000000000000000 ) ;
#22310 = CARTESIAN_POINT ( 'NONE',  ( 4.132952817037856441, 2.031684012687259955, 3.518979934899767237 ) ) ;
#22311 = CIRCLE ( 'NONE', #4253, 5.999999999999998224 ) ;
#22312 = DIRECTION ( 'NONE',  ( 3.885780586188016830E-16, 4.437342591868156373E-31, -1.000000000000000000 ) ) ;
#22313 = CARTESIAN_POINT ( 'NONE',  ( -7.938566201357348362, 4.882486540518906182, -1.249999999999981126 ) ) ;
#22314 = CIRCLE ( 'NONE', #7291, 9.500000000000049738 ) ;
#22315 = CIRCLE ( 'NONE', #12155, 4.500000000000045297 ) ;
#22316 = CARTESIAN_POINT ( 'NONE',  ( -7.500000000000030198, -10.98142396999974935, 8.916666666666721142 ) ) ;
#22317 = EDGE_CURVE ( 'NONE', #10484, #17275, #4730, .T. ) ;
#22318 = CARTESIAN_POINT ( 'NONE',  ( -4.000000000000107470, 2.309401076758546445, -0.4999999999999865663 ) ) ;
#22319 = FACE_OUTER_BOUND ( 'NONE', #7088, .T. ) ;
#22320 = CARTESIAN_POINT ( 'NONE',  ( -7.499999999999965361, -1.999999999999991340, 6.249999999999950262 ) ) ;
#22321 = DIRECTION ( 'NONE',  ( 0.4999999999999998890, 2.286725509617064044E-17, -0.8660254037844387076 ) ) ;
#22322 = EDGE_CURVE ( 'NONE', #14012, #12387, #17869, .T. ) ;
#22323 = CARTESIAN_POINT ( 'NONE',  ( 0.2499999999999828748, 1.999999999999974021, -19.00000000000001066 ) ) ;
#22324 = DIRECTION ( 'NONE',  ( -2.168404344971017743E-16, 1.000000000000000000, 1.287063703585503763E-46 ) ) ;
#22325 = EDGE_CURVE ( 'NONE', #9370, #7710, #12203, .T. ) ;
#22326 = ORIENTED_EDGE ( 'NONE', *, *, #7529, .F. ) ;
#22327 = EDGE_CURVE ( 'NONE', #19695, #6443, #1630, .T. ) ;
#22328 = AXIS2_PLACEMENT_3D ( 'NONE', #12372, #17668, #45 ) ;
#22329 = VERTEX_POINT ( 'NONE', #7171 ) ;
#22330 = ORIENTED_EDGE ( 'NONE', *, *, #9516, .F. ) ;
#22331 = AXIS2_PLACEMENT_3D ( 'NONE', #23125, #16035, #12039 ) ;
#22332 = ORIENTED_EDGE ( 'NONE', *, *, #14867, .F. ) ;
#22333 = CARTESIAN_POINT ( 'NONE',  ( -2.700000000000091216, -2.000000000000043521, 7.500000000000034639 ) ) ;
#22334 = CARTESIAN_POINT ( 'NONE',  ( -6.495190528383328221, 1.387778780781445676E-14, -3.749999999999989342 ) ) ;
#22335 = ORIENTED_EDGE ( 'NONE', *, *, #2396, .F. ) ;
#22336 = FACE_OUTER_BOUND ( 'NONE', #19892, .T. ) ;
#22337 = PLANE ( 'NONE',  #11888 ) ;
#22338 = EDGE_CURVE ( 'NONE', #1155, #6633, #17955, .T. ) ;
#22339 = DIRECTION ( 'NONE',  ( 1.066786462891689527E-26, 6.656013887802287108E-31, 1.000000000000000000 ) ) ;
#22340 = EDGE_CURVE ( 'NONE', #9827, #9220, #12677, .T. ) ;
#22341 = ADVANCED_FACE ( 'NONE', ( #1964 ), #16320, .T. ) ;
#22342 = ORIENTED_EDGE ( 'NONE', *, *, #20305, .T. ) ;
#22343 = CARTESIAN_POINT ( 'NONE',  ( -5.631870895240913555, 35.99999999900384751, -19.26529513898303847 ) ) ;
#22344 = DIRECTION ( 'NONE',  ( -1.000000000000000000, -4.440892098500626162E-16, 5.551115123125782702E-16 ) ) ;
#22345 = FACE_OUTER_BOUND ( 'NONE', #6248, .T. ) ;
#22346 = CARTESIAN_POINT ( 'NONE',  ( -8.718376657154840004, -0.4999999999999867883, 6.820622386031956808 ) ) ;
#22347 = DIRECTION ( 'NONE',  ( -1.000000000000000000, 4.190823558986610327E-31, -1.733449886265890494E-32 ) ) ;
#22348 = AXIS2_PLACEMENT_3D ( 'NONE', #19991, #3984, #21876 ) ;
#22349 = FACE_OUTER_BOUND ( 'NONE', #1461, .T. ) ;
#22350 = VECTOR ( 'NONE', #4497, 1000.000000000000000 ) ;
#22351 = DIRECTION ( 'NONE',  ( 0.000000000000000000, 0.000000000000000000, -1.000000000000000000 ) ) ;
#22352 = CARTESIAN_POINT ( 'NONE',  ( 1.318516776095790322, 3.857556137907070859, 2.806962664615227643E-15 ) ) ;
#22353 = EDGE_CURVE ( 'NONE', #4498, #16689, #13797, .T. ) ;
#22354 = DIRECTION ( 'NONE',  ( 0.000000000000000000, 0.000000000000000000, 1.000000000000000000 ) ) ;
#22355 = ADVANCED_FACE ( 'NONE', ( #7286 ), #23052, .F. ) ;
#22356 = CARTESIAN_POINT ( 'NONE',  ( -89.70000000000059970, 3.200000000000057021, 1.000000000000000888 ) ) ;
#22357 = ORIENTED_EDGE ( 'NONE', *, *, #16566, .T. ) ;
#22358 = CONTEXT_DEPENDENT_SHAPE_REPRESENTATION ( #20223, #15864 ) ;
#22359 = EDGE_LOOP ( 'NONE', ( #8141, #18412, #10487, #9481 ) ) ;
#22360 = AXIS2_PLACEMENT_3D ( 'NONE', #6229, #11861, #1055 ) ;
#22362 = ORIENTED_EDGE ( 'NONE', *, *, #8682, .F. ) ;
#22361 = EDGE_LOOP ( 'NONE', ( #23174, #20388, #15022, #21699 ) ) ;
#22363 = AXIS2_PLACEMENT_3D ( 'NONE', #15774, #10491, #17660 ) ;
#22364 = CYLINDRICAL_SURFACE ( 'NONE', #2760, 3.000000000000000000 ) ;
#22365 = CARTESIAN_POINT ( 'NONE',  ( -5.384454397937119552, 7.656970828559639486E-15, -4.999999999999993783 ) ) ;
#22366 = CARTESIAN_POINT ( 'NONE',  ( 8.954763739086835983, -12.00000000000003908, 6.678571428571491886 ) ) ;
#22367 = ORIENTED_EDGE ( 'NONE', *, *, #19146, .F. ) ;
#22368 = CARTESIAN_POINT ( 'NONE',  ( -4.690415759823517661, -0.7499999999999440448, -2.263420659773247579 ) ) ;
#22369 = CARTESIAN_POINT ( 'NONE',  ( 22.49999999999998224, 2.000000000000001776, -1.250000000000021982 ) ) ;
#22370 = CARTESIAN_POINT ( 'NONE',  ( 4.175813232069142344, -2.061359961916364725, 3.570380186727395433 ) ) ;
#22371 = CARTESIAN_POINT ( 'NONE',  ( 4.050536630291683871, -3.778525289263160225, -0.5912575323401451088 ) ) ;
#22372 = FACE_OUTER_BOUND ( 'NONE', #4843, .T. ) ;
#22373 = DIRECTION ( 'NONE',  ( 0.000000000000000000, 0.000000000000000000, -1.000000000000000000 ) ) ;
#22374 = CARTESIAN_POINT ( 'NONE',  ( 4.330127018922110160, 4.999999999999976907, -7.500000000000003553 ) ) ;
#22375 = SURFACE_SIDE_STYLE ('',( #20264 ) ) ;
#22376 = ADVANCED_FACE ( 'NONE', ( #21640 ), #5515, .F. ) ;
#22377 = DIRECTION ( 'NONE',  ( 1.000000000000000000, 0.000000000000000000, 1.066811114794976679E-26 ) ) ;
#22378 = VECTOR ( 'NONE', #2005, 1000.000000000000114 ) ;
#22379 = PRESENTATION_STYLE_ASSIGNMENT (( #2712 ) ) ;
#22380 = DIRECTION ( 'NONE',  ( -1.134196829589822059E-15, -6.741645191078037727E-32, 1.000000000000000000 ) ) ;
#22381 = CARTESIAN_POINT ( 'NONE',  ( 4.175813232069142344, 2.061359961916364725, -3.570380186727397209 ) ) ;
#22382 = ADVANCED_FACE ( 'NONE', ( #9159 ), #6853, .F. ) ;
#22383 = ORIENTED_EDGE ( 'NONE', *, *, #18183, .F. ) ;
#22385 = ORIENTED_EDGE ( 'NONE', *, *, #19481, .F. ) ;
#22384 = VERTEX_POINT ( 'NONE', #7733 ) ;
#22386 = EDGE_LOOP ( 'NONE', ( #1802, #22367, #16198, #19288 ) ) ;
#22388 = ORIENTED_EDGE ( 'NONE', *, *, #21358, .F. ) ;
#22387 = EDGE_LOOP ( 'NONE', ( #13761, #16746, #10659, #10862 ) ) ;
#22389 = ORIENTED_EDGE ( 'NONE', *, *, #21828, .F. ) ;
#22390 = EDGE_CURVE ( 'NONE', #13674, #9332, #16778, .T. ) ;
#22391 = DIRECTION ( 'NONE',  ( 3.140284632889468553E-31, -1.000000000000000000, 1.734723475976804333E-15 ) ) ;
#22392 = CARTESIAN_POINT ( 'NONE',  ( 88.75737332930594903, -6.527605602963476805, 6.500000000000151879 ) ) ;
#22393 = ORIENTED_EDGE ( 'NONE', *, *, #19042, .T. ) ;
#22394 = CARTESIAN_POINT ( 'NONE',  ( 0.000000000000000000, -3.031088913245536087, -1.750000000000001554 ) ) ;
#22395 = CARTESIAN_POINT ( 'NONE',  ( 0.000000000000000000, 0.000000000000000000, 0.000000000000000000 ) ) ;
#22396 = DIRECTION ( 'NONE',  ( 1.000000000000000000, 0.000000000000000000, 0.000000000000000000 ) ) ;
#22397 = DIRECTION ( 'NONE',  ( 1.000000000000000000, 1.479114197289387852E-30, -2.013525853228518840E-32 ) ) ;
#22398 = CARTESIAN_POINT ( 'NONE',  ( 7.551224464536185899, -2.121331013966567092, 7.234820221745167146 ) ) ;
#22399 = CARTESIAN_POINT ( 'NONE',  ( -12.84999999999999964, -14.00000000000011369, -5.749999999999949374 ) ) ;
#22400 = DIRECTION ( 'NONE',  ( -1.000000000000000000, -2.220446049250313081E-16, 0.000000000000000000 ) ) ;
#22401 = DIRECTION ( 'NONE',  ( 1.000000000000000000, -1.276756478318923119E-15, -1.333893503340774882E-15 ) ) ;
#22402 = CARTESIAN_POINT ( 'NONE',  ( 7.949747468597695210, 47.94974746730969173, -26.50000000000000000 ) ) ;
#22403 = CARTESIAN_POINT ( 'NONE',  ( -0.9238745060512566498, 1.710161125114598279, -4.750000000000025757 ) ) ;
#22404 = LINE ( 'NONE', #6058, #12649 ) ;
#22405 = ORIENTED_EDGE ( 'NONE', *, *, #8695, .F. ) ;
#22406 = VECTOR ( 'NONE', #7163, 1000.000000000000000 ) ;
#22408 = ORIENTED_EDGE ( 'NONE', *, *, #5480, .T. ) ;
#22407 = ORIENTED_EDGE ( 'NONE', *, *, #17293, .T. ) ;
#22409 = ORIENTED_EDGE ( 'NONE', *, *, #19272, .T. ) ;
#22410 = CONICAL_SURFACE ( 'NONE', #11874, 5.560781378645605066, 1.221730476396047704 ) ;
#22411 = ORIENTED_EDGE ( 'NONE', *, *, #1271, .T. ) ;
#22412 = ORIENTED_EDGE ( 'NONE', *, *, #20035, .F. ) ;
#22413 = AXIS2_PLACEMENT_3D ( 'NONE', #22057, #13003, #11108 ) ;
#22414 = ADVANCED_FACE ( 'NONE', ( #4084 ), #11260, .F. ) ;
#22415 = VERTEX_POINT ( 'NONE', #11025 ) ;
#22416 = CARTESIAN_POINT ( 'NONE',  ( 6.000000000291855429, -9.961476088449217059E-10, -5.999999999999998224 ) ) ;
#22417 = DIRECTION ( 'NONE',  ( 0.000000000000000000, 0.000000000000000000, -1.000000000000000000 ) ) ;
#22418 = EDGE_LOOP ( 'NONE', ( #19306, #19362 ) ) ;
#22419 = EDGE_LOOP ( 'NONE', ( #17093, #21210, #7760, #21617 ) ) ;
#22420 = CARTESIAN_POINT ( 'NONE',  ( -55.25320565519150051, 9.020562075079396891E-14, 7.500000000000062172 ) ) ;
#22421 = CARTESIAN_POINT ( 'NONE',  ( 4.175075985190096262, 2.060370777630132544, 3.568666869285558541 ) ) ;
#22422 = DIRECTION ( 'NONE',  ( 0.000000000000000000, -1.000000000000000000, 0.000000000000000000 ) ) ;
#22423 = DIRECTION ( 'NONE',  ( 0.6819983600624957010, 0.7313537016191731244, 7.771699578536735325E-16 ) ) ;
#22424 = CARTESIAN_POINT ( 'NONE',  ( 4.082498951862915781, 4.041451884327383226, -6.134919877127760970E-18 ) ) ;
#22425 = CARTESIAN_POINT ( 'NONE',  ( -7.500000000000007105, -2.645898033750305522, 9.250000000000035527 ) ) ;
#22426 = DIRECTION ( 'NONE',  ( 1.000000000000000000, -9.957992501029406452E-17, -2.655250634480538332E-32 ) ) ;
#22427 = TOROIDAL_SURFACE ( 'NONE', #13779, 2.500000000000002220, 0.5000000000000000000 ) ;
#22428 = CARTESIAN_POINT ( 'NONE',  ( 12.84999999999997300, -1.999999999999998224, 2.549999999999997158 ) ) ;
#22429 = DIRECTION ( 'NONE',  ( 0.7313537016191746787, 0.6819983600624940356, 1.072890437865584409E-16 ) ) ;
#22430 = CIRCLE ( 'NONE', #7045, 5.749999999999992006 ) ;
#22431 = VERTEX_POINT ( 'NONE', #2550 ) ;
#22432 = AXIS2_PLACEMENT_3D ( 'NONE', #20854, #18960, #17175 ) ;
#22433 = CARTESIAN_POINT ( 'NONE',  ( -3.200000000000105427, 1.999999999999911626, -7.500000000000062172 ) ) ;
#22434 = FACE_OUTER_BOUND ( 'NONE', #17931, .T. ) ;
#22436 = ORIENTED_EDGE ( 'NONE', *, *, #16231, .F. ) ;
#22435 = CIRCLE ( 'NONE', #12273, 0.5000000000000004441 ) ;
#22437 = AXIS2_PLACEMENT_3D ( 'NONE', #4452, #22813, #8228 ) ;
#22438 = ORIENTED_EDGE ( 'NONE', *, *, #14695, .F. ) ;
#22439 = ORIENTED_EDGE ( 'NONE', *, *, #8097, .T. ) ;
#22440 = B_SPLINE_CURVE_WITH_KNOTS ( 'NONE', 3,
 ( #1651, #5178, #3306, #1984, #9050 ),
 .UNSPECIFIED., .F., .F.,
 ( 4, 1, 4 ),
 ( 0.000000000000000000, 0.002020725942163690073, 0.004041451884327380145 ),
 .UNSPECIFIED. ) ;
#22441 = EDGE_CURVE ( 'NONE', #3580, #4523, #9389, .T. ) ;
#22442 = DIRECTION ( 'NONE',  ( -0.9878135252003127365, -2.193386639427060722E-16, 0.1556420233463029767 ) ) ;
#22443 = DIRECTION ( 'NONE',  ( -1.000000000000000000, 1.626303258728243832E-16, -1.778091562876213388E-14 ) ) ;
#22444 = ORIENTED_EDGE ( 'NONE', *, *, #16903, .T. ) ;
#22445 = AXIS2_PLACEMENT_3D ( 'NONE', #13398, #11167, #3985 ) ;
#22446 = CARTESIAN_POINT ( 'NONE',  ( 88.75737332930586376, -10.52760560296347947, 6.000000000000165201 ) ) ;
#22447 = FACE_OUTER_BOUND ( 'NONE', #8576, .T. ) ;
#22448 = TOROIDAL_SURFACE ( 'NONE', #15299, 5.500000000000000000, 0.5000000000000000000 ) ;
#22449 = CARTESIAN_POINT ( 'NONE',  ( -4.000000000000087041, -2.309401076758553550, -0.5000000000000004441 ) ) ;
#22450 = EDGE_CURVE ( 'NONE', #14506, #1035, #16657, .T. ) ;
#22451 = DIRECTION ( 'NONE',  ( 0.000000000000000000, 0.000000000000000000, 1.000000000000000000 ) ) ;
#22452 = CARTESIAN_POINT ( 'NONE',  ( 4.052424581287485950, 3.786734753434564560, 0.5771415817954285155 ) ) ;
#22453 = ADVANCED_FACE ( 'NONE', ( #12792 ), #13059, .T. ) ;
#22454 = CIRCLE ( 'NONE', #21724, 2.500000000000015543 ) ;
#22455 = DIRECTION ( 'NONE',  ( 3.032184104443271834E-30, 1.000000000000000000, 4.437342591868167759E-31 ) ) ;
#22456 = ADVANCED_FACE ( 'NONE', ( #18218 ), #2084, .T. ) ;
#22457 = DIRECTION ( 'NONE',  ( 1.000000000000000000, 2.699383410053119644E-30, 3.330669073875432643E-16 ) ) ;
#22458 = DIRECTION ( 'NONE',  ( 0.000000000000000000, 0.000000000000000000, 1.000000000000000000 ) ) ;
#22459 = AXIS2_PLACEMENT_3D ( 'NONE', #14956, #16711, #971 ) ;
#22460 = CARTESIAN_POINT ( 'NONE',  ( 0.000000000000000000, -3.031088913245536087, 1.750000000000003331 ) ) ;
#22461 = CARTESIAN_POINT ( 'NONE',  ( 2.742413778650726108, 1.325747111984056037, 4.749999999999997335 ) ) ;
#22462 = CARTESIAN_POINT ( 'NONE',  ( 2.775557561562891351E-14, 2.999999999999999112, -15.49999999999998579 ) ) ;
#22464 = AXIS2_PLACEMENT_3D ( 'NONE', #14986, #2052, #18518 ) ;
#22463 = CARTESIAN_POINT ( 'NONE',  ( 2.500000000000002220, 3.061616997868386099E-16, -5.574599999999999334 ) ) ;
#22465 = DIRECTION ( 'NONE',  ( -0.5150787536377109399, 0.000000000000000000, 0.8571428571428583165 ) ) ;
#22466 = VECTOR ( 'NONE', #13519, 1000.000000000000000 ) ;
#22467 = AXIS2_PLACEMENT_3D ( 'NONE', #15819, #23018, #5131 ) ;
#22468 = EDGE_CURVE ( 'NONE', #14654, #6, #17342, .T. ) ;
#22469 = EDGE_CURVE ( 'NONE', #800, #9468, #18677, .T. ) ;
#22470 = ITEM_DEFINED_TRANSFORMATION ( 'NONE', 'NONE', #8261,  #22115 ) ;
#22471 = ORIENTED_EDGE ( 'NONE', *, *, #11545, .T. ) ;
#22472 = AXIS2_PLACEMENT_3D ( 'NONE', #8366, #15536, #6380 ) ;
#22474 = VERTEX_POINT ( 'NONE', #18437 ) ;
#22473 = ORIENTED_EDGE ( 'NONE', *, *, #21828, .T. ) ;
#22475 = CIRCLE ( 'NONE', #6341, 2.499999999999993339 ) ;
#22476 = CIRCLE ( 'NONE', #12318, 2.500000000000002220 ) ;
#22477 = DIRECTION ( 'NONE',  ( 2.168404344971005170E-16, 1.000000000000000000, -8.696324126752285467E-47 ) ) ;
#22478 = CYLINDRICAL_SURFACE ( 'NONE', #9597, 2.500000000000000000 ) ;
#22480 = ORIENTED_EDGE ( 'NONE', *, *, #14460, .T. ) ;
#22479 = EDGE_CURVE ( 'NONE', #4649, #17450, #17176, .T. ) ;
#22481 = CARTESIAN_POINT ( 'NONE',  ( 2.966164998648759710, -1.454929939081820445, 4.362451518707887388 ) ) ;
#22482 = DIRECTION ( 'NONE',  ( 0.9706398123736330597, -1.505375731439247434E-16, 0.2405376366294442736 ) ) ;
#22483 = ADVANCED_FACE ( 'NONE', ( #15015 ), #11144, .F. ) ;
#22484 = CARTESIAN_POINT ( 'NONE',  ( -1.747541505913290161, 3.837784562140251765, -3.503702292528905193 ) ) ;
#22485 = LINE ( 'NONE', #4585, #23112 ) ;
#22486 = DIRECTION ( 'NONE',  ( 0.000000000000000000, 0.000000000000000000, -1.000000000000000000 ) ) ;
#22487 = LINE ( 'NONE', #20725, #20470 ) ;
#22488 = ADVANCED_FACE ( 'NONE', ( #16890 ), #6660, .T. ) ;
#22489 = CARTESIAN_POINT ( 'NONE',  ( 0.000000000000000000, 0.000000000000000000, 0.000000000000000000 ) ) ;
#22490 = CARTESIAN_POINT ( 'NONE',  ( -4.295732246213650463, 0.7500000000000505151, -2.802538081657628410 ) ) ;
#22491 = AXIS2_PLACEMENT_3D ( 'NONE', #2435, #16889, #20214 ) ;
#22492 = AXIS2_PLACEMENT_3D ( 'NONE', #18635, #13463, #17087 ) ;
#22493 = CARTESIAN_POINT ( 'NONE',  ( -95.70000000000069917, 0.5000000000000073275, -2.000000000000001776 ) ) ;
#22494 = AXIS2_PLACEMENT_3D ( 'NONE', #6051, #1925, #5938 ) ;
#22495 = FACE_OUTER_BOUND ( 'NONE', #22288, .T. ) ;
#22496 = DIRECTION ( 'NONE',  ( 0.000000000000000000, -1.000000000000000000, 0.000000000000000000 ) ) ;
#22497 = EDGE_LOOP ( 'NONE', ( #7719, #3238, #21267, #21935 ) ) ;
#22498 = EDGE_CURVE ( 'NONE', #19219, #20045, #16416, .T. ) ;
#22499 =( NAMED_UNIT ( * ) PLANE_ANGLE_UNIT ( ) SI_UNIT ( $, .RADIAN. ) );
#22501 = ORIENTED_EDGE ( 'NONE', *, *, #3266, .T. ) ;
#22500 = EDGE_LOOP ( 'NONE', ( #7375, #8696, #5055, #17414 ) ) ;
#22502 = COLOUR_RGB ( '', 0.72549020, 0.75294118, 0.79215686) ;
#22503 = VERTEX_POINT ( 'NONE', #4889 ) ;
#22505 = ORIENTED_EDGE ( 'NONE', *, *, #196, .F. ) ;
#22504 = EDGE_LOOP ( 'NONE', ( #10345, #20994, #16871, #10967, #17004, #16443, #2999 ) ) ;
#22506 = VERTEX_POINT ( 'NONE', #6561 ) ;
#22507 = ADVANCED_FACE ( 'NONE', ( #20682, #15131, #15477 ), #19241, .F. ) ;
#22508 = CARTESIAN_POINT ( 'NONE',  ( -4.000000000000004441, 0.7862748000878052590, -0.03447227762756794461 ) ) ;
#22509 = CYLINDRICAL_SURFACE ( 'NONE', #6583, 0.5000000000000035527 ) ;
#22510 = SURFACE_STYLE_USAGE ( .BOTH. , #15319 ) ;
#22511 = AXIS2_PLACEMENT_3D ( 'NONE', #2409, #14881, #16396 ) ;
#22512 = CYLINDRICAL_SURFACE ( 'NONE', #8895, 2.800000000000000266 ) ;
#22513 = FACE_OUTER_BOUND ( 'NONE', #4358, .T. ) ;
#22514 = CARTESIAN_POINT ( 'NONE',  ( -45.01801948466091829, 6.474873734152938987, -7.500000000000062172 ) ) ;
#22515 = CARTESIAN_POINT ( 'NONE',  ( 7.500000000000006217, -2.428697021684863788, 9.041853041249359180 ) ) ;
#22516 = DIRECTION ( 'NONE',  ( -1.000000000000000000, -2.699383410053119644E-30, -3.330669073875432643E-16 ) ) ;
#22517 = DIRECTION ( 'NONE',  ( 1.550910762415566494E-16, 1.000000000000000000, -8.135128085091684243E-31 ) ) ;
#22518 = STYLED_ITEM ( 'NONE', ( #16141 ), #3025 ) ;
#22519 = FACE_OUTER_BOUND ( 'NONE', #1211, .T. ) ;
#22520 = CARTESIAN_POINT ( 'NONE',  ( -1.839530896101873925, 1.562503694756888439, -4.750000000000024869 ) ) ;
#22521 = B_SPLINE_CURVE_WITH_KNOTS ( 'NONE', 3,
 ( #5390, #12548, #3614, #97, #7268, #14440 ),
 .UNSPECIFIED., .F., .F.,
 ( 4, 2, 4 ),
 ( 0.000000000000000000, 0.002086519881787258016, 0.004173039763574516031 ),
 .UNSPECIFIED. ) ;
#22522 = DIRECTION ( 'NONE',  ( 1.000000000000000000, -1.276756478318922922E-15, 1.333893503340766994E-15 ) ) ;
#22523 = VERTEX_POINT ( 'NONE', #1151 ) ;
#22524 = PRODUCT_DEFINITION_CONTEXT ( 'detailed design', #21574, 'design' ) ;
#22525 = AXIS2_PLACEMENT_3D ( 'NONE', #16237, #21680, #19434 ) ;
#22526 = FILL_AREA_STYLE_COLOUR ( '', #22140 ) ;
#22528 = ORIENTED_EDGE ( 'NONE', *, *, #15426, .T. ) ;
#22527 = ORIENTED_EDGE ( 'NONE', *, *, #8205, .T. ) ;
#22529 = VERTEX_POINT ( 'NONE', #4545 ) ;
#22530 = ORIENTED_EDGE ( 'NONE', *, *, #21604, .T. ) ;
#22531 = AXIS2_PLACEMENT_3D ( 'NONE', #14572, #12692, #7299 ) ;
#22532 = VERTEX_POINT ( 'NONE', #22676 ) ;
#22533 = ADVANCED_FACE ( 'NONE', ( #22434 ), #22448, .T. ) ;
#22534 = AXIS2_PLACEMENT_3D ( 'NONE', #5075, #8717, #15876 ) ;
#22535 = EDGE_LOOP ( 'NONE', ( #22040, #20655 ) ) ;
#22536 = CARTESIAN_POINT ( 'NONE',  ( 3.951447005078449148, 2.357513599190971920, -2.916666666666667407 ) ) ;
#22537 = CARTESIAN_POINT ( 'NONE',  ( 30.00000000029184832, -0.5000000009961480529, -39.00000000000000000 ) ) ;
#22538 = ORIENTED_EDGE ( 'NONE', *, *, #1601, .T. ) ;
#22539 = ORIENTED_EDGE ( 'NONE', *, *, #3757, .F. ) ;
#22540 = CARTESIAN_POINT ( 'NONE',  ( 108.9540049198142242, -11.33354449810611264, -6.000000000000074607 ) ) ;
#22541 = EDGE_CURVE ( 'NONE', #15424, #7856, #15240, .T. ) ;
#22542 = LINE ( 'NONE', #15803, #7981 ) ;
#22543 = CARTESIAN_POINT ( 'NONE',  ( -4.857225732735059864E-14, 4.500000000000059508, -17.50000000000000711 ) ) ;
#22544 = DIRECTION ( 'NONE',  ( -4.440892098500625669E-16, 1.000000000000000000, 1.224646799147351975E-16 ) ) ;
#22545 = CARTESIAN_POINT ( 'NONE',  ( -45.01801948466092540, 6.474873734152931881, -8.000000000000062172 ) ) ;
#22546 = CARTESIAN_POINT ( 'NONE',  ( -7.802869476033403195, -11.64353246333686265, 7.917139222843291968 ) ) ;
#22547 = CARTESIAN_POINT ( 'NONE',  ( -7.920269128372687817, -13.36773923605932168, 7.713069291591535759 ) ) ;
#22548 = LINE ( 'NONE', #15358, #5988 ) ;
#22549 = TOROIDAL_SURFACE ( 'NONE', #16885, 9.499999999999998224, 0.5000000000000000000 ) ;
#22550 = CARTESIAN_POINT ( 'NONE',  ( 22.50000000000003908, 4.500000000000031974, -0.2499999999999967526 ) ) ;
#22551 = CARTESIAN_POINT ( 'NONE',  ( -6.000000000000116351, 4.799999999999957190, -7.500000000000062172 ) ) ;
#22552 = VERTEX_POINT ( 'NONE', #18910 ) ;
#22553 = SURFACE_SIDE_STYLE ('',( #3145 ) ) ;
#22554 = DIRECTION ( 'NONE',  ( 1.000000000000000000, 3.254448077276381206E-32, 1.066788928082016908E-26 ) ) ;
#22555 = DIRECTION ( 'NONE',  ( 0.000000000000000000, 0.000000000000000000, -1.000000000000000000 ) ) ;
#22556 = VERTEX_POINT ( 'NONE', #13841 ) ;
#22557 = VERTEX_POINT ( 'NONE', #15364 ) ;
#22558 = VERTEX_POINT ( 'NONE', #8082 ) ;
#22559 = ORIENTED_EDGE ( 'NONE', *, *, #4345, .T. ) ;
#22560 = DIRECTION ( 'NONE',  ( 1.000000000000000000, -1.550910762415513985E-16, -3.012982189080959477E-32 ) ) ;
#22561 = CARTESIAN_POINT ( 'NONE',  ( 119.5756419024615269, -11.00000000000006573, 6.000000000000081712 ) ) ;
#22562 = ORIENTED_EDGE ( 'NONE', *, *, #4336, .T. ) ;
#22563 = AXIS2_PLACEMENT_3D ( 'NONE', #16576, #7436, #19789 ) ;
#22564 = FACE_OUTER_BOUND ( 'NONE', #19009, .T. ) ;
#22565 = LINE ( 'NONE', #17367, #6637 ) ;
#22566 = LINE ( 'NONE', #6451, #17736 ) ;
#22567 = CARTESIAN_POINT ( 'NONE',  ( -4.896882909245229953, 36.38534960922553552, -18.98204752465805356 ) ) ;
#22568 = FACE_OUTER_BOUND ( 'NONE', #11374, .T. ) ;
#22569 = CARTESIAN_POINT ( 'NONE',  ( -7.756475484083187766, -0.06559517125032440776, 7.145789564688667994 ) ) ;
#22570 = PRODUCT_RELATED_PRODUCT_CATEGORY ( 'part', '', ( #7073 ) ) ;
#22571 = CARTESIAN_POINT ( 'NONE',  ( -25.39999999999989555, 2.775557561562891351E-14, 6.938893903907228378E-14 ) ) ;
#22572 = CARTESIAN_POINT ( 'NONE',  ( -87.15000000000055991, -9.060110299520993284E-14, -2.000000000000002220 ) ) ;
#22573 = DIRECTION ( 'NONE',  ( 1.550910762415566494E-16, 1.000000000000000000, -8.135128085091684243E-31 ) ) ;
#22574 = LINE ( 'NONE', #7991, #10045 ) ;
#22575 = DIRECTION ( 'NONE',  ( 0.000000000000000000, 0.000000000000000000, 1.000000000000000000 ) ) ;
#22576 = EDGE_CURVE ( 'NONE', #19223, #8999, #8203, .T. ) ;
#22577 = DIRECTION ( 'NONE',  ( 0.000000000000000000, 0.000000000000000000, -1.000000000000000000 ) ) ;
#22578 = AXIS2_PLACEMENT_3D ( 'NONE', #19529, #12102, #11882 ) ;
#22579 = ORIENTED_EDGE ( 'NONE', *, *, #10023, .T. ) ;
#22580 = ADVANCED_FACE ( 'NONE', ( #19131 ), #1403, .T. ) ;
#22581 = ITEM_DEFINED_TRANSFORMATION ( 'NONE', 'NONE', #21423,  #22115 ) ;
#22582 = ORIENTED_EDGE ( 'NONE', *, *, #15592, .T. ) ;
#22584 = ORIENTED_EDGE ( 'NONE', *, *, #16585, .F. ) ;
#22583 = ORIENTED_EDGE ( 'NONE', *, *, #9360, .F. ) ;
#22585 = DIRECTION ( 'NONE',  ( 1.000000000000000000, -2.168404344971005170E-16, 1.203141491611682442E-30 ) ) ;
#22586 = DIRECTION ( 'NONE',  ( -1.000000000000000000, -1.479114197289397135E-31, -5.916456789157588541E-31 ) ) ;
#22587 = DIRECTION ( 'NONE',  ( 1.000000000000000000, 0.000000000000000000, 0.000000000000000000 ) ) ;
#22588 = ORIENTED_EDGE ( 'NONE', *, *, #3610, .F. ) ;
#22589 = AXIS2_PLACEMENT_3D ( 'NONE', #21767, #16447, #12458 ) ;
#22590 = COLOUR_RGB ( '', 0.08235294, 0.09019608, 0.10196078) ;
#22591 = FACE_OUTER_BOUND ( 'NONE', #21111, .T. ) ;
#22592 = LINE ( 'NONE', #11414, #14673 ) ;
#22593 = DIRECTION ( 'NONE',  ( -1.000000000000000000, -2.699383410053119644E-30, -3.330669073875432643E-16 ) ) ;
#22595 = ADVANCED_FACE ( 'NONE', ( #1034 ), #11949, .F. ) ;
#22594 = FACE_OUTER_BOUND ( 'NONE', #17396, .T. ) ;
#22596 = DIRECTION ( 'NONE',  ( -1.333893503340774882E-15, -2.778352770573747380E-17, -1.000000000000000000 ) ) ;
#22597 = DIRECTION ( 'NONE',  ( 2.013525853228507892E-32, 6.902532920683810383E-31, -1.000000000000000000 ) ) ;
#22598 = CARTESIAN_POINT ( 'NONE',  ( -2.499999999999993339, 2.886579864025407005E-14, 17.49999999999997513 ) ) ;
#22599 = DIRECTION ( 'NONE',  ( 1.000000000000000000, -2.633062418893351796E-15, 0.000000000000000000 ) ) ;
#22600 = EDGE_CURVE ( 'NONE', #16375, #9602, #22818, .T. ) ;
#22601 = FACE_OUTER_BOUND ( 'NONE', #9012, .T. ) ;
#22602 = CARTESIAN_POINT ( 'NONE',  ( -42.54314575050782565, -4.800000000000064659, -8.000000000000007105 ) ) ;
#22603 = ORIENTED_EDGE ( 'NONE', *, *, #17293, .F. ) ;
#22604 = EDGE_CURVE ( 'NONE', #882, #3485, #10801, .T. ) ;
#22605 = DIRECTION ( 'NONE',  ( -0.7296441571687836136, -0.6838270277705141842, 1.414107600981053804E-16 ) ) ;
#22606 = TOROIDAL_SURFACE ( 'NONE', #9088, 2.500000000000000000, 0.5000000000000000000 ) ;
#22607 = CIRCLE ( 'NONE', #10938, 0.5000000000000029976 ) ;
#22608 = ADVANCED_FACE ( 'NONE', ( #12054 ), #16050, .T. ) ;
#22610 = VERTEX_POINT ( 'NONE', #17355 ) ;
#22609 = ORIENTED_EDGE ( 'NONE', *, *, #13004, .F. ) ;
#22611 = EDGE_CURVE ( 'NONE', #4863, #10470, #18317, .T. ) ;
#22612 = ORIENTED_EDGE ( 'NONE', *, *, #2329, .F. ) ;
#22614 = ORIENTED_EDGE ( 'NONE', *, *, #3490, .F. ) ;
#22613 = VERTEX_POINT ( 'NONE', #1266 ) ;
#22615 = ORIENTED_EDGE ( 'NONE', *, *, #10614, .T. ) ;
#22616 = DIRECTION ( 'NONE',  ( -1.066786462891689527E-26, -6.656013887802287108E-31, -1.000000000000000000 ) ) ;
#22617 = DIRECTION ( 'NONE',  ( -3.885780586188016830E-16, -4.437342591868156373E-31, 1.000000000000000000 ) ) ;
#22618 =( NAMED_UNIT ( * ) PLANE_ANGLE_UNIT ( ) SI_UNIT ( $, .RADIAN. ) );
#22619 = LINE ( 'NONE', #12135, #9246 ) ;
#22620 = DIRECTION ( 'NONE',  ( 2.172745813409349776E-17, -1.000000000000000000, 1.309377075419428048E-16 ) ) ;
#22621 = ADVANCED_FACE ( 'NONE', ( #22787 ), #4426, .T. ) ;
#22622 = CARTESIAN_POINT ( 'NONE',  ( 30.00000000029184832, 2.999999999003851503, -39.00000000000000000 ) ) ;
#22623 = EDGE_CURVE ( 'NONE', #6539, #6214, #21337, .T. ) ;
#22624 = EDGE_CURVE ( 'NONE', #1329, #15019, #14189, .T. ) ;
#22625 = FACE_OUTER_BOUND ( 'NONE', #1945, .T. ) ;
#22626 = CARTESIAN_POINT ( 'NONE',  ( -8.326672684688674053E-14, -2.000000000000029310, 8.000000000000076383 ) ) ;
#22627 = CARTESIAN_POINT ( 'NONE',  ( 7.324400034341884691, -2.232976452217586782, 7.601326208249607141 ) ) ;
#22628 = VECTOR ( 'NONE', #22073, 1000.000000000000000 ) ;
#22629 = CARTESIAN_POINT ( 'NONE',  ( -2.682243648011765735, -3.070208061305350622, -0.04852650426608514506 ) ) ;
#22630 = CARTESIAN_POINT ( 'NONE',  ( 6.500000000000339284, 2.500000000000141220, -6.499999999999950262 ) ) ;
#22631 = CIRCLE ( 'NONE', #4969, 2.500000000000003553 ) ;
#22632 = SPHERICAL_SURFACE ( 'NONE', #20954, 0.5000000000000000000 ) ;
#22633 = CARTESIAN_POINT ( 'NONE',  ( 3.000000000291852764, 42.99999999900385461, -45.00000000000000000 ) ) ;
#22634 = CARTESIAN_POINT ( 'NONE',  ( -6.359599319592073030, 13.97158350606811617, -27.86358591318706246 ) ) ;
#22635 = EDGE_CURVE ( 'NONE', #4139, #7855, #7059, .T. ) ;
#22636 = DIRECTION ( 'NONE',  ( -1.000000000000000000, -2.168404344971017743E-16, 1.780660105995169760E-30 ) ) ;
#22637 = PRODUCT_DEFINITION_SHAPE ( 'NONE', 'NONE',  #23270 ) ;
#22638 = ORIENTED_EDGE ( 'NONE', *, *, #13748, .T. ) ;
#22639 = EDGE_CURVE ( 'NONE', #8580, #9470, #20207, .T. ) ;
#22641 = VERTEX_POINT ( 'NONE', #8898 ) ;
#22640 = ORIENTED_EDGE ( 'NONE', *, *, #6444, .F. ) ;
#22642 = EDGE_CURVE ( 'NONE', #13378, #4065, #1599, .T. ) ;
#22643 = ORIENTED_EDGE ( 'NONE', *, *, #3061, .T. ) ;
#22644 = ORIENTED_EDGE ( 'NONE', *, *, #18747, .T. ) ;
#22645 = AXIS2_PLACEMENT_3D ( 'NONE', #1929, #12406, #2165 ) ;
#22646 = CIRCLE ( 'NONE', #10238, 0.5000000000000004441 ) ;
#22647 = ORIENTED_EDGE ( 'NONE', *, *, #19324, .T. ) ;
#22648 = VECTOR ( 'NONE', #13508, 1000.000000000000000 ) ;
#22649 = AXIS2_PLACEMENT_3D ( 'NONE', #9005, #21252, #5118 ) ;
#22650 = AXIS2_PLACEMENT_3D ( 'NONE', #15073, #3918, #2501 ) ;
#22651 = ORIENTED_EDGE ( 'NONE', *, *, #13683, .F. ) ;
#22652 = FACE_BOUND ( 'NONE', #18106, .T. ) ;
#22653 = ADVANCED_BREP_SHAPE_REPRESENTATION ( '', ( #20836, #22115 ), #712 ) ;
#22654 = LINE ( 'NONE', #18774, #7238 ) ;
#22655 = ORIENTED_EDGE ( 'NONE', *, *, #11801, .F. ) ;
#22656 = EDGE_LOOP ( 'NONE', ( #11926, #17930, #20626, #21389 ) ) ;
#22657 = DIRECTION ( 'NONE',  ( -0.7313537016191746787, -0.6819983600624940356, -1.072890437865584409E-16 ) ) ;
#22658 = CARTESIAN_POINT ( 'NONE',  ( 0.000000000000000000, 3.031088913245536087, 1.749999999999998002 ) ) ;
#22659 = CARTESIAN_POINT ( 'NONE',  ( 4.071447262713884463, 2.020725942163681399, 3.499999999999996003 ) ) ;
#22660 = CARTESIAN_POINT ( 'NONE',  ( 42.50000000000014921, 8.000000000000003553, -14.99999999999998579 ) ) ;
#22661 = DIRECTION ( 'NONE',  ( 3.885780586188016830E-16, 4.437342591868156373E-31, -1.000000000000000000 ) ) ;
#22662 = FACE_OUTER_BOUND ( 'NONE', #8298, .T. ) ;
#22663 = CARTESIAN_POINT ( 'NONE',  ( -4.749999999999944933, 3.738560049591893758E-14, -3.000000000000002665 ) ) ;
#22664 = AXIS2_PLACEMENT_3D ( 'NONE', #10180, #17346, #15810 ) ;
#22665 = CIRCLE ( 'NONE', #13643, 3.000000000000011102 ) ;
#22666 = VECTOR ( 'NONE', #10377, 1000.000000000000000 ) ;
#22667 = CARTESIAN_POINT ( 'NONE',  ( -7.499999999999992895, -8.000000000000044409, 6.250000000000005329 ) ) ;
#22668 = AXIS2_PLACEMENT_3D ( 'NONE', #19706, #14409, #10976 ) ;
#22669 = EDGE_CURVE ( 'NONE', #22298, #16918, #13814, .T. ) ;
#22670 = FACE_OUTER_BOUND ( 'NONE', #2904, .T. ) ;
#22671 = AXIS2_PLACEMENT_3D ( 'NONE', #6857, #1684, #17313 ) ;
#22672 = EDGE_LOOP ( 'NONE', ( #13812, #9854, #17094, #1857 ) ) ;
#22673 = CIRCLE ( 'NONE', #17000, 7.000000000000089706 ) ;
#22674 =( LENGTH_UNIT ( ) NAMED_UNIT ( * ) SI_UNIT ( .MILLI., .METRE. ) );
#22675 = DIRECTION ( 'NONE',  ( 0.000000000000000000, 0.000000000000000000, 1.000000000000000000 ) ) ;
#22676 = CARTESIAN_POINT ( 'NONE',  ( -50.65685424949281668, 3.200000000000022382, 7.500000000000034639 ) ) ;
#22677 = VERTEX_POINT ( 'NONE', #17842 ) ;
#22678 = ADVANCED_FACE ( 'NONE', ( #19727 ), #2917, .T. ) ;
#22679 = ORIENTED_EDGE ( 'NONE', *, *, #19894, .F. ) ;
#22680 = VERTEX_POINT ( 'NONE', #19365 ) ;
#22681 = VERTEX_POINT ( 'NONE', #3602 ) ;
#22682 = ORIENTED_EDGE ( 'NONE', *, *, #21956, .F. ) ;
#22683 = CARTESIAN_POINT ( 'NONE',  ( 111.3116192909783422, -9.818697260249892977, 6.500000000000012434 ) ) ;
#22684 = CARTESIAN_POINT ( 'NONE',  ( -67.28510754798017501, -1.040834085586084257E-13, 12.22107821754960000 ) ) ;
#22685 = VECTOR ( 'NONE', #5977, 1000.000000000000000 ) ;
#22686 = ORIENTED_EDGE ( 'NONE', *, *, #13997, .T. ) ;
#22687 = AXIS2_PLACEMENT_3D ( 'NONE', #15034, #11738, #22223 ) ;
#22688 = CARTESIAN_POINT ( 'NONE',  ( 12.49999999999995914, 0.2500000000000002220, -14.25000000000000355 ) ) ;
#22689 = AXIS2_PLACEMENT_3D ( 'NONE', #17397, #8477, #22830 ) ;
#22690 = FACE_OUTER_BOUND ( 'NONE', #9849, .T. ) ;
#22691 = CARTESIAN_POINT ( 'NONE',  ( -6.999999999708142795, 38.99999999900385461, -26.50000000000000000 ) ) ;
#22692 = VECTOR ( 'NONE', #19171, 1000.000000000000000 ) ;
#22693 = MECHANICAL_DESIGN_GEOMETRIC_PRESENTATION_REPRESENTATION (  '', ( #1640 ), #140 ) ;
#22694 = ADVANCED_FACE ( 'NONE', ( #3484 ), #21386, .T. ) ;
#22695 = FACE_OUTER_BOUND ( 'NONE', #13869, .T. ) ;
#22696 = CARTESIAN_POINT ( 'NONE',  ( 88.75737332930597745, -13.02760560296348302, -6.000000000000039968 ) ) ;
#22697 = DIRECTION ( 'NONE',  ( -2.013525853228507892E-32, -6.902532920683810383E-31, 1.000000000000000000 ) ) ;
#22698 = LINE ( 'NONE', #819, #21246 ) ;
#22699 = LINE ( 'NONE', #1169, #21698 ) ;
#22700 = DIRECTION ( 'NONE',  ( 0.000000000000000000, 0.000000000000000000, 1.000000000000000000 ) ) ;
#22701 = DIRECTION ( 'NONE',  ( -9.693647360340828445E-26, 0.000000000000000000, 1.000000000000000000 ) ) ;
#22702 = DIRECTION ( 'NONE',  ( -2.013525853228507892E-32, -6.902532920683810383E-31, 1.000000000000000000 ) ) ;
#22703 = VECTOR ( 'NONE', #12764, 1000.000000000000000 ) ;
#22704 = CARTESIAN_POINT ( 'NONE',  ( 6.938893903907228378E-15, 4.618802153517023612, -5.000000000000000888 ) ) ;
#22705 = CIRCLE ( 'NONE', #22331, 0.5000000000000028866 ) ;
#22706 = ORIENTED_EDGE ( 'NONE', *, *, #10990, .F. ) ;
#22708 = ORIENTED_EDGE ( 'NONE', *, *, #7728, .T. ) ;
#22707 = ORIENTED_EDGE ( 'NONE', *, *, #7654, .T. ) ;
#22709 = FACE_OUTER_BOUND ( 'NONE', #21763, .T. ) ;
#22710 = CARTESIAN_POINT ( 'NONE',  ( -4.499999999708154341, 35.99999999900384751, -25.50000000000000000 ) ) ;
#22711 = EDGE_CURVE ( 'NONE', #4165, #4144, #17568, .T. ) ;
#22712 = DIRECTION ( 'NONE',  ( 8.438582421954109416E-32, 0.000000000000000000, 1.000000000000000000 ) ) ;
#22713 = VECTOR ( 'NONE', #17312, 1000.000000000000000 ) ;
#22714 = ORIENTED_EDGE ( 'NONE', *, *, #17604, .T. ) ;
#22715 = DIRECTION ( 'NONE',  ( 1.333893503340774882E-15, 2.778352770573747380E-17, 1.000000000000000000 ) ) ;
#22716 = AXIS2_PLACEMENT_3D ( 'NONE', #1763, #19650, #21660 ) ;
#22717 = DIRECTION ( 'NONE',  ( 0.7071067811865507924, 0.7071067811865441310, 2.121016688166342479E-16 ) ) ;
#22718 = DIRECTION ( 'NONE',  ( 0.7313537016191735685, -0.6819983600624951459, 3.923113172947598083E-16 ) ) ;
#22719 = CARTESIAN_POINT ( 'NONE',  ( 26.09619407800442659, 29.09619407671642222, -19.00000000000000355 ) ) ;
#22720 = DIRECTION ( 'NONE',  ( 1.000000000000000000, -1.424116703980815236E-16, -2.931272055834072749E-32 ) ) ;
#22721 = FACE_OUTER_BOUND ( 'NONE', #16945, .T. ) ;
#22722 = CARTESIAN_POINT ( 'NONE',  ( -12.84999999999998721, -1.999999999999998224, -5.749999999999991118 ) ) ;
#22723 = DIRECTION ( 'NONE',  ( 2.013525853228507892E-32, 6.902532920683810383E-31, -1.000000000000000000 ) ) ;
#22724 =( NAMED_UNIT ( * ) PLANE_ANGLE_UNIT ( ) SI_UNIT ( $, .RADIAN. ) );
#22725 = EDGE_CURVE ( 'NONE', #4606, #12089, #8549, .T. ) ;
#22726 = ORIENTED_EDGE ( 'NONE', *, *, #18018, .F. ) ;
#22727 = AXIS2_PLACEMENT_3D ( 'NONE', #7306, #15866, #14473 ) ;
#22728 = CARTESIAN_POINT ( 'NONE',  ( -29.81695455880978329, 89.54066614605915220, 34.16570243528391160 ) ) ;
#22729 = VECTOR ( 'NONE', #37, 1000.000000000000000 ) ;
#22731 = VERTEX_POINT ( 'NONE', #5010 ) ;
#22730 = ORIENTED_EDGE ( 'NONE', *, *, #18726, .T. ) ;
#22732 = UNCERTAINTY_MEASURE_WITH_UNIT (LENGTH_MEASURE( 1.000000000000000082E-05 ), #4279, 'distance_accuracy_value', 'NONE');
#22733 = ORIENTED_EDGE ( 'NONE', *, *, #5664, .F. ) ;
#22734 = EDGE_CURVE ( 'NONE', #6728, #4783, #5259, .T. ) ;
#22736 = ORIENTED_EDGE ( 'NONE', *, *, #15859, .T. ) ;
#22735 = EDGE_LOOP ( 'NONE', ( #9245, #399, #8085, #8115 ) ) ;
#22737 = B_SPLINE_CURVE_WITH_KNOTS ( 'NONE', 3,
 ( #19255, #1838, #8910, #21153, #10439, #8674 ),
 .UNSPECIFIED., .F., .F.,
 ( 4, 2, 4 ),
 ( 0.001997790223414142811, 0.003382245482991528586, 0.004766700742568914795 ),
 .UNSPECIFIED. ) ;
#22738 = LINE ( 'NONE', #4954, #5397 ) ;
#22739 = CARTESIAN_POINT ( 'NONE',  ( 12.49999999999992362, 1.250000000000015099, -14.25000000000000178 ) ) ;
#22740 = EDGE_CURVE ( 'NONE', #16729, #8301, #7083, .T. ) ;
#22741 = DIRECTION ( 'NONE',  ( 1.454462294001240516E-30, 1.000000000000000000, 0.000000000000000000 ) ) ;
#22742 = DIRECTION ( 'NONE',  ( -2.013525853228507892E-32, -6.902532920683810383E-31, 1.000000000000000000 ) ) ;
#22743 = CARTESIAN_POINT ( 'NONE',  ( -8.260108127873330375, -2.109168607890870906, 7.249251683976359217 ) ) ;
#22744 = CONICAL_SURFACE ( 'NONE', #12590, 7.499999999999998224, 1.308996938995750092 ) ;
#22745 = CARTESIAN_POINT ( 'NONE',  ( 3.951447005078450037, 1.347150628109125670, 3.499999999999999112 ) ) ;
#22746 = EDGE_CURVE ( 'NONE', #7130, #9737, #3315, .T. ) ;
#22747 = CARTESIAN_POINT ( 'NONE',  ( -64.00000000000045475, 6.245004513516505540E-14, -1.999999999999974021 ) ) ;
#22748 = VECTOR ( 'NONE', #13186, 1000.000000000000000 ) ;
#22749 = ADVANCED_FACE ( 'NONE', ( #3263 ), #8662, .T. ) ;
#22750 = CARTESIAN_POINT ( 'NONE',  ( -89.70000000000055707, -3.200000000000091660, -1.999999999999946265 ) ) ;
#22751 = DIRECTION ( 'NONE',  ( 0.000000000000000000, 0.000000000000000000, 1.000000000000000000 ) ) ;
#22752 = EDGE_CURVE ( 'NONE', #2725, #14653, #15924, .T. ) ;
#22753 = FACE_OUTER_BOUND ( 'NONE', #8492, .T. ) ;
#22754 = CARTESIAN_POINT ( 'NONE',  ( -7.713464495932024434, -12.17135227947844278, 8.131426806228684967 ) ) ;
#22755 = DIRECTION ( 'NONE',  ( 2.775557561562884572E-17, 0.000000000000000000, 1.000000000000000000 ) ) ;
#22756 = CARTESIAN_POINT ( 'NONE',  ( 2.775557561562891351E-14, 2.499999999999998668, -0.4999999999999865663 ) ) ;
#22757 = ORIENTED_EDGE ( 'NONE', *, *, #7975, .F. ) ;
#22758 = AXIS2_PLACEMENT_3D ( 'NONE', #20722, #17168, #13426 ) ;
#22760 = ORIENTED_EDGE ( 'NONE', *, *, #14327, .F. ) ;
#22759 = ORIENTED_EDGE ( 'NONE', *, *, #13478, .T. ) ;
#22761 = VERTEX_POINT ( 'NONE', #2749 ) ;
#22762 = EDGE_CURVE ( 'NONE', #21726, #23235, #6317, .T. ) ;
#22763 = EDGE_LOOP ( 'NONE', ( #19756, #15625, #20740, #17785, #20003, #11112, #4254, #509 ) ) ;
#22764 = ORIENTED_EDGE ( 'NONE', *, *, #19433, .F. ) ;
#22765 = EDGE_LOOP ( 'NONE', ( #8351, #22173, #4085, #1300, #10142, #20886, #17927, #17719 ) ) ;
#22766 = CYLINDRICAL_SURFACE ( 'NONE', #16663, 0.4999999999999987232 ) ;
#22767 = AXIS2_PLACEMENT_3D ( 'NONE', #2857, #17196, #19201 ) ;
#22768 = DIRECTION ( 'NONE',  ( 8.438582421954109416E-32, 0.000000000000000000, 1.000000000000000000 ) ) ;
#22769 = EDGE_CURVE ( 'NONE', #7130, #4606, #19453, .T. ) ;
#22770 = EDGE_LOOP ( 'NONE', ( #1492, #18972, #4492, #4702 ) ) ;
#22771 = CARTESIAN_POINT ( 'NONE',  ( 0.1381419387119531828, -1.355287006778843173, -3.500000000000035527 ) ) ;
#22772 = PLANE ( 'NONE',  #21139 ) ;
#22773 = STYLED_ITEM ( 'NONE', ( #469 ), #21131 ) ;
#22774 = ADVANCED_FACE ( 'NONE', ( #1231 ), #2639, .T. ) ;
#22775 = CARTESIAN_POINT ( 'NONE',  ( -55.05572809000126711, 2.700000000000021938, -7.500000000000034639 ) ) ;
#22776 = CARTESIAN_POINT ( 'NONE',  ( 6.999999999999992006, -8.000000000000003553, 12.25000000000001066 ) ) ;
#22777 = CARTESIAN_POINT ( 'NONE',  ( 0.2499999999999898137, 6.938893903907228378E-14, -17.00000000000000711 ) ) ;
#22778 = FACE_BOUND ( 'NONE', #775, .T. ) ;
#22779 = EDGE_CURVE ( 'NONE', #16059, #16601, #18992, .T. ) ;
#22780 = CARTESIAN_POINT ( 'NONE',  ( 42.50000000000014921, 8.000000000000003553, 2.000000000000071054 ) ) ;
#22781 = DIRECTION ( 'NONE',  ( 0.5000000000000066613, 0.8660254037844348218, -0.000000000000000000 ) ) ;
#22782 = AXIS2_PLACEMENT_3D ( 'NONE', #8308, #1254, #13721 ) ;
#22783 = DIRECTION ( 'NONE',  ( 1.734723475976813750E-16, 1.000000000000000000, -3.469446951953607484E-15 ) ) ;
#22784 = CARTESIAN_POINT ( 'NONE',  ( -4.330127018922179438, 4.999999999999976907, -7.500000000000000000 ) ) ;
#22785 = EDGE_LOOP ( 'NONE', ( #1096, #7343, #7695, #11712 ) ) ;
#22786 = DIRECTION ( 'NONE',  ( 0.8571428571428572063, -4.467596029561073242E-15, -0.5150787536377126052 ) ) ;
#22787 = FACE_OUTER_BOUND ( 'NONE', #12235, .T. ) ;
#22789 = ORIENTED_EDGE ( 'NONE', *, *, #5591, .T. ) ;
#22788 = EDGE_LOOP ( 'NONE', ( #22760, #17008, #7967, #18530 ) ) ;
#22790 = EDGE_CURVE ( 'NONE', #16175, #19930, #22286, .T. ) ;
#22791 = VECTOR ( 'NONE', #416, 1000.000000000000000 ) ;
#22792 = ORIENTED_EDGE ( 'NONE', *, *, #4025, .T. ) ;
#22793 = EDGE_LOOP ( 'NONE', ( #20351, #4605, #2972, #20807 ) ) ;
#22794 = EDGE_LOOP ( 'NONE', ( #1427, #16465, #17040, #17606 ) ) ;
#22795 = FACE_BOUND ( 'NONE', #10597, .T. ) ;
#22796 = ORIENTED_EDGE ( 'NONE', *, *, #4507, .T. ) ;
#22797 = CARTESIAN_POINT ( 'NONE',  ( 7.980290731945706817, -0.6082991440336660283, 7.616182555102799512 ) ) ;
#22798 = EDGE_CURVE ( 'NONE', #18554, #7256, #4627, .T. ) ;
#22799 = DIRECTION ( 'NONE',  ( 0.000000000000000000, 0.000000000000000000, 1.000000000000000000 ) ) ;
#22800 = DIRECTION ( 'NONE',  ( -3.070652698126929572E-17, -1.000000000000000000, 2.869019762633796499E-16 ) ) ;
#22801 = VERTEX_POINT ( 'NONE', #15446 ) ;
#22802 = VECTOR ( 'NONE', #21509, 1000.000000000000000 ) ;
#22803 = DIRECTION ( 'NONE',  ( -3.944304526105059903E-31, -0.5000000000000014433, -0.8660254037844378194 ) ) ;
#22804 = CARTESIAN_POINT ( 'NONE',  ( 12.84999999999997300, -12.00000000000011191, -6.249999999999936051 ) ) ;
#22805 = ADVANCED_FACE ( 'NONE', ( #22171, #2870 ), #10047, .T. ) ;
#22806 = CARTESIAN_POINT ( 'NONE',  ( -8.496394830447121294, -0.03251735406441521453, 6.998792816379902249 ) ) ;
#22807 = ADVANCED_FACE ( 'NONE', ( #20409 ), #15334, .F. ) ;
#22808 = VECTOR ( 'NONE', #4594, 1000.000000000000000 ) ;
#22809 = CARTESIAN_POINT ( 'NONE',  ( 0.000000000000000000, 0.000000000000000000, 0.000000000000000000 ) ) ;
#22810 = CARTESIAN_POINT ( 'NONE',  ( 118.0000000000018190, -6.500000000000061284, -6.000000000000012434 ) ) ;
#22811 = CARTESIAN_POINT ( 'NONE',  ( -7.499999999999978684, -8.000000000000024869, 10.74999999999999645 ) ) ;
#22812 = CIRCLE ( 'NONE', #10388, 6.500000000000075495 ) ;
#22813 = DIRECTION ( 'NONE',  ( -0.9878135252003120703, -1.331202777560448839E-30, 0.1556420233463080560 ) ) ;
#22814 = CARTESIAN_POINT ( 'NONE',  ( -0.6666666666666698493, 4.233901974057265427, -3.300726591567082036 ) ) ;
#22815 = LINE ( 'NONE', #22704, #19462 ) ;
#22816 = ORIENTED_EDGE ( 'NONE', *, *, #20439, .F. ) ;
#22817 = ORIENTED_EDGE ( 'NONE', *, *, #174, .F. ) ;
#22818 = CIRCLE ( 'NONE', #1789, 0.4999999999999995559 ) ;
#22819 = CARTESIAN_POINT ( 'NONE',  ( 0.000000000000000000, 2.775557561562891351E-14, 17.49999999999997513 ) ) ;
#22820 = CIRCLE ( 'NONE', #14172, 1.300000000000009592 ) ;
#22822 = ORIENTED_EDGE ( 'NONE', *, *, #20091, .T. ) ;
#22821 = VERTEX_POINT ( 'NONE', #8288 ) ;
#22823 = DIRECTION ( 'NONE',  ( 1.000000000000000000, 1.479114197289397135E-31, 5.916456789157588541E-31 ) ) ;
#22824 = EDGE_CURVE ( 'NONE', #19389, #2652, #14210, .T. ) ;
#22825 = ORIENTED_EDGE ( 'NONE', *, *, #8652, .F. ) ;
#22826 = CARTESIAN_POINT ( 'NONE',  ( 108.2426266706970353, -10.52760560296359138, -6.000000000000019540 ) ) ;
#22827 = FACE_OUTER_BOUND ( 'NONE', #544, .T. ) ;
#22828 = CIRCLE ( 'NONE', #2926, 2.500000000000014655 ) ;
#22829 = ORIENTED_EDGE ( 'NONE', *, *, #2342, .T. ) ;
#22830 = DIRECTION ( 'NONE',  ( 0.000000000000000000, 0.000000000000000000, 1.000000000000000000 ) ) ;
#22831 = LINE ( 'NONE', #20718, #12346 ) ;
#22832 = DIRECTION ( 'NONE',  ( -4.003208021484906984E-16, 7.395570986447125806E-32, 1.000000000000000000 ) ) ;
#22833 = PRODUCT_DEFINITION_SHAPE ( 'NONE', 'NONE',  #21853 ) ;
#22834 = CIRCLE ( 'NONE', #12679, 0.5000000000000004441 ) ;
#22835 = EDGE_CURVE ( 'NONE', #16377, #13233, #4428, .T. ) ;
#22836 = CARTESIAN_POINT ( 'NONE',  ( -0.5000000000000975886, 1.999999999999932498, -7.500000000000007105 ) ) ;
#22837 = DIRECTION ( 'NONE',  ( -2.168404344970994323E-16, 1.000000000000000000, -1.577721810442023611E-30 ) ) ;
#22838 = AXIS2_PLACEMENT_3D ( 'NONE', #3650, #1656, #18114 ) ;
#22839 = CARTESIAN_POINT ( 'NONE',  ( -2.681483223904238322, 3.070647092368425479, -5.600000000000002309 ) ) ;
#22840 = CARTESIAN_POINT ( 'NONE',  ( -45.56568542494959928, -0.5000000000000698330, -8.000000000000035527 ) ) ;
#22841 = CARTESIAN_POINT ( 'NONE',  ( 124.5000000000018900, -13.52760560296373171, 6.500000000000068390 ) ) ;
#22842 = AXIS2_PLACEMENT_3D ( 'NONE', #14041, #14159, #8866 ) ;
#22843 = CARTESIAN_POINT ( 'NONE',  ( 6.500000000000227374, 3.000000000000169198, 4.163336342344337027E-14 ) ) ;
#22844 = AXIS2_PLACEMENT_3D ( 'NONE', #18453, #9630, #20462 ) ;
#22845 = ORIENTED_EDGE ( 'NONE', *, *, #13900, .F. ) ;
#22846 = EDGE_CURVE ( 'NONE', #6039, #2116, #11915, .T. ) ;
#22847 = AXIS2_PLACEMENT_3D ( 'NONE', #4626, #3347, #10386 ) ;
#22848 = DIRECTION ( 'NONE',  ( 0.000000000000000000, -1.387778780781445676E-16, -0.9999999999999998890 ) ) ;
#22850 = EDGE_LOOP ( 'NONE', ( #1998, #17630, #11629, #9168 ) ) ;
#22849 = VERTEX_POINT ( 'NONE', #16860 ) ;
#22851 = ORIENTED_EDGE ( 'NONE', *, *, #20909, .T. ) ;
#22853 = ORIENTED_EDGE ( 'NONE', *, *, #7627, .T. ) ;
#22852 = ORIENTED_EDGE ( 'NONE', *, *, #7340, .T. ) ;
#22854 = EDGE_LOOP ( 'NONE', ( #20484, #11210, #20191, #20076 ) ) ;
#22855 = CARTESIAN_POINT ( 'NONE',  ( -12.85000000000001386, -12.00000000000008704, -2.549999999999958966 ) ) ;
#22856 = DIRECTION ( 'NONE',  ( -1.000000000000000000, 0.000000000000000000, 1.734723475976805319E-15 ) ) ;
#22857 = CARTESIAN_POINT ( 'NONE',  ( 36.00000000029184832, -9.961476088449217059E-10, -39.00000000000000000 ) ) ;
#22858 = CARTESIAN_POINT ( 'NONE',  ( -4.330127018922234505, -2.775557561562891351E-14, -7.499999999999989342 ) ) ;
#22859 = AXIS2_PLACEMENT_3D ( 'NONE', #14442, #21158, #99 ) ;
#22860 = CARTESIAN_POINT ( 'NONE',  ( -7.000000000000005329, -0.7870719649792564665, 9.239863038076329360 ) ) ;
#22861 = CARTESIAN_POINT ( 'NONE',  ( -8.129778652391257410, -1.578738987863637089, 7.405931224841305394 ) ) ;
#22862 = VECTOR ( 'NONE', #3546, 1000.000000000000000 ) ;
#22863 = DIRECTION ( 'NONE',  ( -1.000000000000000000, -2.699383410053119293E-30, -4.336808689941968432E-16 ) ) ;
#22864 = DIRECTION ( 'NONE',  ( -1.000000000000000000, -2.220446049250297797E-16, 0.000000000000000000 ) ) ;
#22865 = AXIS2_PLACEMENT_3D ( 'NONE', #14350, #10820, #21435 ) ;
#22866 = CARTESIAN_POINT ( 'NONE',  ( 0.2500000000000036637, 2.000000000000001776, -17.00000000000000711 ) ) ;
#22867 = LINE ( 'NONE', #21100, #21133 ) ;
#22868 = CARTESIAN_POINT ( 'NONE',  ( -42.54314575050799618, 3.999999999999996447, 8.000000000000035527 ) ) ;
#22869 = DIRECTION ( 'NONE',  ( 0.000000000000000000, -1.000000000000000000, 0.000000000000000000 ) ) ;
#22870 = CARTESIAN_POINT ( 'NONE',  ( -4.197477534772400709, 0.8522413273724812610, -3.505042416683278983 ) ) ;
#22871 = APPLICATION_CONTEXT ( 'automotive_design' ) ;
#22872 = CARTESIAN_POINT ( 'NONE',  ( 37.00000000000011369, 10.49999999999999822, -6.499999999999950262 ) ) ;
#22873 = STYLED_ITEM ( 'NONE', ( #6780 ), #5834 ) ;
#22874 = ORIENTED_EDGE ( 'NONE', *, *, #448, .T. ) ;
#22875 = EDGE_CURVE ( 'NONE', #1072, #5239, #19830, .T. ) ;
#22877 = EDGE_LOOP ( 'NONE', ( #10959, #13627, #3362, #9044 ) ) ;
#22876 = ORIENTED_EDGE ( 'NONE', *, *, #12201, .F. ) ;
#22878 = VERTEX_POINT ( 'NONE', #23115 ) ;
#22879 = AXIS2_PLACEMENT_3D ( 'NONE', #5280, #12323, #7285 ) ;
#22880 = PRODUCT_DEFINITION ( 'UNKNOWN', '', #21783, #4161 ) ;
#22881 = EDGE_CURVE ( 'NONE', #18297, #20512, #10738, .T. ) ;
#22882 = ORIENTED_EDGE ( 'NONE', *, *, #3219, .F. ) ;
#22883 = VECTOR ( 'NONE', #16420, 1000.000000000000000 ) ;
#22884 = AXIS2_PLACEMENT_3D ( 'NONE', #11472, #434, #11248 ) ;
#22885 = ORIENTED_EDGE ( 'NONE', *, *, #17990, .F. ) ;
#22886 = ADVANCED_FACE ( 'NONE', ( #6996 ), #11188, .F. ) ;
#22887 = ORIENTED_EDGE ( 'NONE', *, *, #3938, .F. ) ;
#22888 = CARTESIAN_POINT ( 'NONE',  ( -42.54314575050793934, 7.999999999999992895, 8.000000000000035527 ) ) ;
#22889 = DIRECTION ( 'NONE',  ( -1.000000000000000000, 0.000000000000000000, 0.000000000000000000 ) ) ;
#22890 = ORIENTED_EDGE ( 'NONE', *, *, #13863, .F. ) ;
#22891 = CARTESIAN_POINT ( 'NONE',  ( -7.980290731945705041, -13.39170085596635573, 7.616182555102821716 ) ) ;
#22892 = CARTESIAN_POINT ( 'NONE',  ( 0.000000000000000000, -14.99999999999997513, -1.387778780781445676E-14 ) ) ;
#22893 = DIRECTION ( 'NONE',  ( 3.254448077146059901E-32, 1.000000000000000000, 6.409494854920712161E-31 ) ) ;
#22894 = CARTESIAN_POINT ( 'NONE',  ( -6.959227345695446765, 36.00023956896081501, -26.49293639998818506 ) ) ;
#22895 = CARTESIAN_POINT ( 'NONE',  ( 2.773872027544998636E-14, 11.99999999999999645, 2.500000000000007105 ) ) ;
#22896 = DIRECTION ( 'NONE',  ( 1.000000000000000000, 2.220446049250314560E-16, 0.000000000000000000 ) ) ;
#22897 = DIRECTION ( 'NONE',  ( -3.885780586188016830E-16, -4.437342591868156373E-31, 1.000000000000000000 ) ) ;
#22898 = EDGE_CURVE ( 'NONE', #8200, #19103, #13449, .T. ) ;
#22899 = CYLINDRICAL_SURFACE ( 'NONE', #1909, 0.5000000000000038858 ) ;
#22900 = AXIS2_PLACEMENT_3D ( 'NONE', #23263, #8661, #8783 ) ;
#22901 = FACE_BOUND ( 'NONE', #19003, .T. ) ;
#22902 = CARTESIAN_POINT ( 'NONE',  ( 0.2499999999999655276, 2.000000000000015543, -2.000000000000001776 ) ) ;
#22903 = DIRECTION ( 'NONE',  ( 0.000000000000000000, 1.000000000000000000, 0.000000000000000000 ) ) ;
#22904 = ORIENTED_EDGE ( 'NONE', *, *, #15391, .F. ) ;
#22905 = EDGE_CURVE ( 'NONE', #16513, #10482, #3688, .T. ) ;
#22906 = DIRECTION ( 'NONE',  ( -2.172745813409349776E-17, 1.000000000000000000, -1.309377075419428048E-16 ) ) ;
#22907 = DIRECTION ( 'NONE',  ( 1.066786462891689527E-26, 6.656013887802287108E-31, 1.000000000000000000 ) ) ;
#22908 = CIRCLE ( 'NONE', #11255, 4.000000000000045297 ) ;
#22910 = ORIENTED_EDGE ( 'NONE', *, *, #5491, .F. ) ;
#22909 = VERTEX_POINT ( 'NONE', #23232 ) ;
#22911 =( GEOMETRIC_REPRESENTATION_CONTEXT ( 3 ) GLOBAL_UNCERTAINTY_ASSIGNED_CONTEXT ( ( #12643 ) ) GLOBAL_UNIT_ASSIGNED_CONTEXT ( ( #8412, #2996, #19217 ) ) REPRESENTATION_CONTEXT ( 'NONE', 'WORKASPACE' ) );
#22912 = ADVANCED_FACE ( 'NONE', ( #6629 ), #13178, .F. ) ;
#22913 = ORIENTED_EDGE ( 'NONE', *, *, #17277, .T. ) ;
#22914 = EDGE_CURVE ( 'NONE', #21618, #13307, #16809, .T. ) ;
#22915 = EDGE_LOOP ( 'NONE', ( #17966, #19338, #933 ) ) ;
#22916 = EDGE_LOOP ( 'NONE', ( #18242, #17711, #2520, #11499 ) ) ;
#22917 = DIRECTION ( 'NONE',  ( -3.469446951953611428E-15, 1.000000000000000000, -3.469446951953610245E-15 ) ) ;
#22918 = CARTESIAN_POINT ( 'NONE',  ( -45.37157287525410254, -6.828427124746218269, 8.000000000000035527 ) ) ;
#22919 = CARTESIAN_POINT ( 'NONE',  ( -8.697224362268011433, 6.938893903907228378E-15, 6.249999999999992006 ) ) ;
#22920 = DIRECTION ( 'NONE',  ( -5.598259082250079541E-17, 1.000000000000000000, -6.162975822039171151E-32 ) ) ;
#22921 = FACE_BOUND ( 'NONE', #14772, .T. ) ;
#22922 = DIRECTION ( 'NONE',  ( 0.000000000000000000, -1.000000000000000000, 0.000000000000000000 ) ) ;
#22923 = CYLINDRICAL_SURFACE ( 'NONE', #22097, 0.5000000000000004441 ) ;
#22924 = AXIS2_PLACEMENT_3D ( 'NONE', #16957, #18853, #2737 ) ;
#22925 = CARTESIAN_POINT ( 'NONE',  ( -8.115139842999401054, -0.1079360712687468249, 7.423524081915970463 ) ) ;
#22926 = EDGE_CURVE ( 'NONE', #18025, #7684, #10072, .T. ) ;
#22927 = AXIS2_PLACEMENT_3D ( 'NONE', #22964, #6725, #1664 ) ;
#22928 = EDGE_CURVE ( 'NONE', #8955, #10857, #5947, .T. ) ;
#22929 = DIRECTION ( 'NONE',  ( 1.000000000000000000, 4.440892098500626162E-16, -5.551115123125782702E-16 ) ) ;
#22930 = ADVANCED_FACE ( 'NONE', ( #4858 ), #13918, .F. ) ;
#22931 = CARTESIAN_POINT ( 'NONE',  ( -8.954763739086866181, -13.50000000000003553, 6.678571428571478563 ) ) ;
#22932 = CARTESIAN_POINT ( 'NONE',  ( 2.499999999999993339, 2.695151429079059169E-14, 17.49999999999997513 ) ) ;
#22933 = LINE ( 'NONE', #3730, #18308 ) ;
#22934 = CARTESIAN_POINT ( 'NONE',  ( -0.5469614295398264048, 4.303013824934858178, -3.535263753543724352 ) ) ;
#22935 = CARTESIAN_POINT ( 'NONE',  ( -12.84999999999999964, -2.000000000000001776, 2.549999999999997158 ) ) ;
#22936 = DIRECTION ( 'NONE',  ( -2.220446049250313081E-16, 1.000000000000000000, -7.025792437124636392E-31 ) ) ;
#22937 = VERTEX_POINT ( 'NONE', #19689 ) ;
#22938 = EDGE_CURVE ( 'NONE', #9093, #14699, #13074, .T. ) ;
#22939 = EDGE_CURVE ( 'NONE', #16094, #5042, #4050, .T. ) ;
#22940 = CONICAL_SURFACE ( 'NONE', #15039, 2.249999999999996003, 0.7853981633974439491 ) ;
#22941 = EDGE_LOOP ( 'NONE', ( #2149, #7538, #17102, #6189 ) ) ;
#22942 = EDGE_CURVE ( 'NONE', #4090, #12296, #2938, .T. ) ;
#22943 = ADVANCED_FACE ( 'NONE', ( #21439 ), #12352, .T. ) ;
#22944 = SHAPE_REPRESENTATION ( 'slotted pan head screw_bsi_BS EN ISO 1580 - M5 x 25 - 25N', ( #22115 ), #14985 ) ;
#22945 = CARTESIAN_POINT ( 'NONE',  ( 1.199999999999992628, 0.000000000000000000, 0.000000000000000000 ) ) ;
#22947 = ORIENTED_EDGE ( 'NONE', *, *, #12246, .F. ) ;
#22946 = ORIENTED_EDGE ( 'NONE', *, *, #3386, .F. ) ;
#22948 = DIRECTION ( 'NONE',  ( 0.5150787536377134934, 0.000000000000000000, 0.8571428571428567622 ) ) ;
#22949 = ORIENTED_EDGE ( 'NONE', *, *, #13980, .F. ) ;
#22950 = DIRECTION ( 'NONE',  ( -0.000000000000000000, -0.000000000000000000, 1.000000000000000000 ) ) ;
#22951 = DIRECTION ( 'NONE',  ( 0.000000000000000000, 1.000000000000000000, 0.000000000000000000 ) ) ;
#22952 = DIRECTION ( 'NONE',  ( -1.333893503340774882E-15, -2.778352770573747380E-17, -1.000000000000000000 ) ) ;
#22953 = ORIENTED_EDGE ( 'NONE', *, *, #8180, .T. ) ;
#22954 = CARTESIAN_POINT ( 'NONE',  ( -4.330127018922248716, 4.689110867544532546, 7.500000000000007105 ) ) ;
#22955 = LINE ( 'NONE', #17049, #5231 ) ;
#22956 = PLANE ( 'NONE',  #10178 ) ;
#22957 = CARTESIAN_POINT ( 'NONE',  ( 3.806834918298617865, -1.387778780781445676E-14, 3.499999999999940936 ) ) ;
#22958 = CARTESIAN_POINT ( 'NONE',  ( 3.973110223767149840, -2.262799480050941678E-11, -3.565797985667468417 ) ) ;
#22959 = DIRECTION ( 'NONE',  ( -0.7071067811865507924, -0.7071067811865444641, 1.064654809502291460E-15 ) ) ;
#22960 = DIRECTION ( 'NONE',  ( 0.000000000000000000, 0.000000000000000000, -1.000000000000000000 ) ) ;
#22961 = SURFACE_STYLE_FILL_AREA ( #12113 ) ;
#22962 = EDGE_CURVE ( 'NONE', #17095, #9471, #20743, .T. ) ;
#22963 = ORIENTED_EDGE ( 'NONE', *, *, #9477, .F. ) ;
#22964 = CARTESIAN_POINT ( 'NONE',  ( -57.51225780766258566, -8.340516433293984733, 49.76570243528392723 ) ) ;
#22966 = ORIENTED_EDGE ( 'NONE', *, *, #197, .T. ) ;
#22965 = ORIENTED_EDGE ( 'NONE', *, *, #7395, .F. ) ;
#22967 = EDGE_CURVE ( 'NONE', #7393, #19198, #9479, .T. ) ;
#22968 = ORIENTED_EDGE ( 'NONE', *, *, #14775, .F. ) ;
#22970 = EDGE_LOOP ( 'NONE', ( #13231, #8632 ) ) ;
#22969 = ORIENTED_EDGE ( 'NONE', *, *, #1757, .T. ) ;
#22971 = CIRCLE ( 'NONE', #13219, 3.499999999999999556 ) ;
#22972 = CARTESIAN_POINT ( 'NONE',  ( -95.70000000000065654, -1.318389841742373392E-13, -2.000000000000029310 ) ) ;
#22973 = LINE ( 'NONE', #6733, #22729 ) ;
#22974 = CARTESIAN_POINT ( 'NONE',  ( 6.999999999999978684, -8.000000000000003553, 11.74999999999999645 ) ) ;
#22975 = CARTESIAN_POINT ( 'NONE',  ( -6.999999999708156118, 6.999999999003851947, -26.00000000000000000 ) ) ;
#22976 = FACE_OUTER_BOUND ( 'NONE', #16029, .T. ) ;
#22977 = DIRECTION ( 'NONE',  ( 0.000000000000000000, 3.382522293539642681E-32, 1.000000000000000000 ) ) ;
#22978 = CARTESIAN_POINT ( 'NONE',  ( 4.295266925971481520, -0.7499999999999386047, -2.803037596611578586 ) ) ;
#22979 = CARTESIAN_POINT ( 'NONE',  ( 119.5756419024615838, -11.00000000000006573, -6.500000000000075495 ) ) ;
#22980 = CARTESIAN_POINT ( 'NONE',  ( -64.00000000000038369, -3.200000000000081446, -2.000000000000029310 ) ) ;
#22981 = EDGE_CURVE ( 'NONE', #14201, #19371, #5576, .T. ) ;
#22982 = DIRECTION ( 'NONE',  ( 0.7071067811865507924, 0.7071067811865444641, -1.064654809502291460E-15 ) ) ;
#22983 = CARTESIAN_POINT ( 'NONE',  ( 2.775557561562891351E-14, 10.99999999999998579, -2.133974596215532316 ) ) ;
#22984 = CARTESIAN_POINT ( 'NONE',  ( 3.000000000291852764, 42.99999999900385461, -29.00000000000000355 ) ) ;
#22985 = CARTESIAN_POINT ( 'NONE',  ( -42.54314575050793934, 7.499999999999992895, 7.500000000000062172 ) ) ;
#22986 = CARTESIAN_POINT ( 'NONE',  ( -7.595478965369722779, -11.97605770252013180, 8.489833260407468885 ) ) ;
#22987 = AXIS2_PLACEMENT_3D ( 'NONE', #15587, #2890, #13830 ) ;
#22988 = VECTOR ( 'NONE', #12926, 1000.000000000000227 ) ;
#22989 = CARTESIAN_POINT ( 'NONE',  ( 4.330127018922110160, 4.689110867544560080, 7.499999999999985789 ) ) ;
#22990 = CARTESIAN_POINT ( 'NONE',  ( 29.00000000029184832, 16.99999999900385461, -18.50000000000000355 ) ) ;
#22991 = EDGE_LOOP ( 'NONE', ( #19952, #21361, #22887, #13333 ) ) ;
#22993 = VERTEX_POINT ( 'NONE', #3789 ) ;
#22992 = ORIENTED_EDGE ( 'NONE', *, *, #2937, .F. ) ;
#22994 = ORIENTED_EDGE ( 'NONE', *, *, #14140, .T. ) ;
#22995 = ORIENTED_EDGE ( 'NONE', *, *, #18284, .T. ) ;
#22996 = VERTEX_POINT ( 'NONE', #391 ) ;
#22997 = EDGE_LOOP ( 'NONE', ( #92, #16801, #15714, #20706 ) ) ;
#22998 = DIRECTION ( 'NONE',  ( -3.944304526105060779E-31, -0.8660254037844379305, -0.5000000000000012212 ) ) ;
#22999 = VECTOR ( 'NONE', #13193, 1000.000000000000000 ) ;
#23000 = AXIS2_PLACEMENT_3D ( 'NONE', #15727, #15492, #12190 ) ;
#23001 = DIRECTION ( 'NONE',  ( -0.9878135252003126254, 5.551115123125605208E-17, 0.1556420233463029767 ) ) ;
#23002 = ORIENTED_EDGE ( 'NONE', *, *, #18416, .T. ) ;
#23003 = CARTESIAN_POINT ( 'NONE',  ( 37.86602540378461157, 11.00000000000000000, -10.86602540378450676 ) ) ;
#23004 = CARTESIAN_POINT ( 'NONE',  ( 3.344563996438205677, 2.687817229851463985, -5.441324518471517102 ) ) ;
#23005 = EDGE_CURVE ( 'NONE', #15339, #22298, #11184, .T. ) ;
#23006 = CARTESIAN_POINT ( 'NONE',  ( 4.000000000000003553, -0.3902508023145571658, -5.599999999999998757 ) ) ;
#23007 = DIRECTION ( 'NONE',  ( 1.000000000000000000, 2.699383410053119644E-30, 3.330669073875432643E-16 ) ) ;
#23008 = CARTESIAN_POINT ( 'NONE',  ( -7.607945571813282903, -0.8975439866888990093, 8.443122311927307777 ) ) ;
#23009 = FACE_OUTER_BOUND ( 'NONE', #16717, .T. ) ;
#23010 = CARTESIAN_POINT ( 'NONE',  ( 22.49999999999998934, 4.250000000000017764, -19.00000000000001421 ) ) ;
#23011 = DIRECTION ( 'NONE',  ( -0.7071067811865454633, 0.7071067811865497932, 0.000000000000000000 ) ) ;
#23012 = CARTESIAN_POINT ( 'NONE',  ( 37.68301270189238750, 11.00000000000000355, -10.50000000000005329 ) ) ;
#23013 = AXIS2_PLACEMENT_3D ( 'NONE', #15900, #12610, #12843 ) ;
#23014 = CARTESIAN_POINT ( 'NONE',  ( 2.775557561562891351E-14, 11.00000000000000000, -6.499999999999950262 ) ) ;
#23015 = CARTESIAN_POINT ( 'NONE',  ( -7.955953741309929939, -1.644172503818049025, 7.654083333123823607 ) ) ;
#23016 = ORIENTED_EDGE ( 'NONE', *, *, #16522, .T. ) ;
#23017 = DIRECTION ( 'NONE',  ( -1.000000000000000000, -1.479114197289387852E-30, 2.013525853228518840E-32 ) ) ;
#23018 = DIRECTION ( 'NONE',  ( 3.330669073875432643E-16, 4.437342591868153746E-31, -1.000000000000000000 ) ) ;
#23019 = CIRCLE ( 'NONE', #12868, 4.750000000000013323 ) ;
#23021 = EDGE_LOOP ( 'NONE', ( #11825, #11120, #395, #19902 ) ) ;
#23020 = ORIENTED_EDGE ( 'NONE', *, *, #4648, .F. ) ;
#23022 = EDGE_CURVE ( 'NONE', #7393, #12162, #12682, .T. ) ;
#23023 = AXIS2_PLACEMENT_3D ( 'NONE', #16408, #22071, #11345 ) ;
#23024 = CIRCLE ( 'NONE', #7240, 2.549999999999998934 ) ;
#23025 = AXIS2_PLACEMENT_3D ( 'NONE', #11368, #11489, #13737 ) ;
#23026 = ORIENTED_EDGE ( 'NONE', *, *, #15455, .F. ) ;
#23027 = VERTEX_POINT ( 'NONE', #269 ) ;
#23028 = VERTEX_POINT ( 'NONE', #13084 ) ;
#23029 = CARTESIAN_POINT ( 'NONE',  ( 25.15499999999999403, 8.456305733849119291E-32, 2.499999999999996891 ) ) ;
#23030 = EDGE_CURVE ( 'NONE', #4132, #23243, #20974, .T. ) ;
#23031 = CARTESIAN_POINT ( 'NONE',  ( 4.498682454207562909E-16, -14.99999999999997335, -4.750000000000026645 ) ) ;
#23032 = PRESENTATION_LAYER_ASSIGNMENT (  '', '', ( #17365 ) ) ;
#23033 = B_SPLINE_CURVE_WITH_KNOTS ( 'NONE', 3,
 ( #15202, #22044, #15320, #527, #18626, #14975 ),
 .UNSPECIFIED., .F., .F.,
 ( 4, 2, 4 ),
 ( 0.01308430721348209647, 0.01410661710602281738, 0.01512892699856353829 ),
 .UNSPECIFIED. ) ;
#23034 = DIRECTION ( 'NONE',  ( 0.000000000000000000, -1.000000000000000000, 2.168404344971006896E-16 ) ) ;
#23035 = CARTESIAN_POINT ( 'NONE',  ( -2.099999999999999645, 2.571758278209440971E-16, -0.2800830152838856835 ) ) ;
#23036 = CARTESIAN_POINT ( 'NONE',  ( 0.1388410611046271281, -2.351840044243068917, 2.926493552096038897 ) ) ;
#23037 = ADVANCED_FACE ( 'NONE', ( #7449 ), #7560, .F. ) ;
#23038 = DIRECTION ( 'NONE',  ( 1.000000000000000000, 0.000000000000000000, 4.336808689942013792E-16 ) ) ;
#23039 = AXIS2_PLACEMENT_3D ( 'NONE', #4120, #20017, #21900 ) ;
#23040 = FACE_OUTER_BOUND ( 'NONE', #6908, .T. ) ;
#23041 = CARTESIAN_POINT ( 'NONE',  ( -95.20000000000065654, 3.200000000000015277, -2.000000000000001776 ) ) ;
#23042 = CIRCLE ( 'NONE', #2736, 0.5000000000000038858 ) ;
#23043 = DIRECTION ( 'NONE',  ( 1.000000000000000000, -4.440892098500658702E-16, 0.000000000000000000 ) ) ;
#23044 = CIRCLE ( 'NONE', #8395, 5.560781378645605066 ) ;
#23045 = DIRECTION ( 'NONE',  ( 2.220446049250313081E-16, -1.000000000000000000, 7.025792437124636392E-31 ) ) ;
#23046 = DIRECTION ( 'NONE',  ( -1.000000000000000000, 0.000000000000000000, 0.000000000000000000 ) ) ;
#23047 = EDGE_CURVE ( 'NONE', #9172, #2421, #16066, .T. ) ;
#23048 = EDGE_CURVE ( 'NONE', #3062, #7230, #8951, .T. ) ;
#23049 = CARTESIAN_POINT ( 'NONE',  ( 0.000000000000000000, -1.750000000000001554, 0.000000000000000000 ) ) ;
#23050 = LINE ( 'NONE', #6804, #11913 ) ;
#23051 = FACE_OUTER_BOUND ( 'NONE', #12353, .T. ) ;
#23052 = CYLINDRICAL_SURFACE ( 'NONE', #21701, 2.999999999999995559 ) ;
#23053 = ORIENTED_EDGE ( 'NONE', *, *, #15321, .F. ) ;
#23054 = CONICAL_SURFACE ( 'NONE', #133, 2.060000000000013820, 0.9599310885968820317 ) ;
#23055 = AXIS2_PLACEMENT_3D ( 'NONE', #3703, #1928, #14181 ) ;
#23056 = EDGE_LOOP ( 'NONE', ( #15652, #12572, #2693 ) ) ;
#23057 = CIRCLE ( 'NONE', #11770, 0.7500000000000000000 ) ;
#23058 = AXIS2_PLACEMENT_3D ( 'NONE', #22945, #10803, #1745 ) ;
#23059 = EDGE_CURVE ( 'NONE', #3643, #84, #21917, .T. ) ;
#23060 = TOROIDAL_SURFACE ( 'NONE', #19679, 7.882182279042408979, 2.500000000000000000 ) ;
#23061 = CARTESIAN_POINT ( 'NONE',  ( -5.471017171483509856, 36.21317998574328811, -26.11735242742819452 ) ) ;
#23062 =( GEOMETRIC_REPRESENTATION_CONTEXT ( 3 ) GLOBAL_UNCERTAINTY_ASSIGNED_CONTEXT ( ( #16595 ) ) GLOBAL_UNIT_ASSIGNED_CONTEXT ( ( #15433, #21330, #13906 ) ) REPRESENTATION_CONTEXT ( 'NONE', 'WORKASPACE' ) );
#23063 = EDGE_CURVE ( 'NONE', #13739, #16369, #22022, .T. ) ;
#23064 = EDGE_CURVE ( 'NONE', #22431, #8991, #20590, .T. ) ;
#23066 = VERTEX_POINT ( 'NONE', #7337 ) ;
#23065 = EDGE_LOOP ( 'NONE', ( #19514, #12946 ) ) ;
#23067 = CARTESIAN_POINT ( 'NONE',  ( -7.500000000000007105, -5.999999999999987566, 10.25000000000000888 ) ) ;
#23068 = DIRECTION ( 'NONE',  ( -5.916456789157588541E-31, 3.382522293539642681E-32, 1.000000000000000000 ) ) ;
#23069 = CARTESIAN_POINT ( 'NONE',  ( 3.000000000000008438, -8.030144996622774890E-16, 4.749999999999979572 ) ) ;
#23070 = CARTESIAN_POINT ( 'NONE',  ( 2.775557561562891351E-14, 2.999999999999999112, -15.49999999999998579 ) ) ;
#23071 = ORIENTED_EDGE ( 'NONE', *, *, #14240, .T. ) ;
#23072 = PLANE ( 'NONE',  #18544 ) ;
#23073 = CARTESIAN_POINT ( 'NONE',  ( 6.500000000000005329, -13.52760560296348302, -6.500000000000075495 ) ) ;
#23074 = EDGE_CURVE ( 'NONE', #20880, #700, #11078, .T. ) ;
#23075 = CARTESIAN_POINT ( 'NONE',  ( -12.85000000000004228, -1.499999999999997780, -6.249999999999977796 ) ) ;
#23076 = CARTESIAN_POINT ( 'NONE',  ( -7.735962016526146456, -13.93008758169059824, 7.174192622767023408 ) ) ;
#23077 = CYLINDRICAL_SURFACE ( 'NONE', #5457, 0.5000000000000004441 ) ;
#23078 = AXIS2_PLACEMENT_3D ( 'NONE', #4300, #13373, #15360 ) ;
#23079 = DIRECTION ( 'NONE',  ( 1.000000000000000000, 2.699383410053119644E-30, 3.330669073875432643E-16 ) ) ;
#23080 = EDGE_CURVE ( 'NONE', #1098, #17626, #9328, .T. ) ;
#23081 = VECTOR ( 'NONE', #14752, 1000.000000000000000 ) ;
#23082 = CARTESIAN_POINT ( 'NONE',  ( 24.75000000000000355, 2.000000000000029310, -2.000000000000005329 ) ) ;
#23083 = CARTESIAN_POINT ( 'NONE',  ( 12.84999999999999964, -12.50000000000011191, -6.249999999999921840 ) ) ;
#23084 = VECTOR ( 'NONE', #12063, 1000.000000000000000 ) ;
#23086 = EDGE_CURVE ( 'NONE', #21118, #10966, #18383, .T. ) ;
#23085 = DIRECTION ( 'NONE',  ( -0.000000000000000000, -0.000000000000000000, -1.000000000000000000 ) ) ;
#23087 =( NAMED_UNIT ( * ) SI_UNIT ( $, .STERADIAN. ) SOLID_ANGLE_UNIT ( ) );
#23088 = ORIENTED_EDGE ( 'NONE', *, *, #17247, .F. ) ;
#23090 = ORIENTED_EDGE ( 'NONE', *, *, #8108, .F. ) ;
#23089 = EDGE_LOOP ( 'NONE', ( #17098, #1702, #19350, #3001 ) ) ;
#23091 = ORIENTED_EDGE ( 'NONE', *, *, #1182, .T. ) ;
#23092 = AXIS2_PLACEMENT_3D ( 'NONE', #21340, #15897, #21681 ) ;
#23094 = ORIENTED_EDGE ( 'NONE', *, *, #11086, .F. ) ;
#23093 = EDGE_LOOP ( 'NONE', ( #7344, #10771, #781, #2144 ) ) ;
#23095 = CLOSED_SHELL ( 'NONE', ( #15134, #11065, #18757, #530, #15834, #16427, #12418 ) ) ;
#23096 = AXIS2_PLACEMENT_3D ( 'NONE', #20263, #499, #16814 ) ;
#23097 = DIRECTION ( 'NONE',  ( -1.000000000000000000, -1.479114197289388027E-30, 2.013525853228518840E-32 ) ) ;
#23098 = AXIS2_PLACEMENT_3D ( 'NONE', #12271, #8422, #12397 ) ;
#23099 = DIRECTION ( 'NONE',  ( 1.454462294001240516E-30, 1.000000000000000000, 7.888609052210128564E-31 ) ) ;
#23100 = FACE_OUTER_BOUND ( 'NONE', #15547, .T. ) ;
#23101 = CARTESIAN_POINT ( 'NONE',  ( -67.40537636629485974, -2.700000000000125855, 12.70639812373639010 ) ) ;
#23102 = CYLINDRICAL_SURFACE ( 'NONE', #1361, 0.5000000000000004441 ) ;
#23103 = EDGE_CURVE ( 'NONE', #21697, #12036, #14562, .T. ) ;
#23104 = CARTESIAN_POINT ( 'NONE',  ( -3.999999999708153453, 38.99999999900385461, -29.00000000000000355 ) ) ;
#23105 = DIRECTION ( 'NONE',  ( 0.7071067811865506814, -0.7071067811865445751, 6.116169571546738730E-15 ) ) ;
#23106 = DIRECTION ( 'NONE',  ( -1.000000000000000000, 0.000000000000000000, 0.000000000000000000 ) ) ;
#23107 = CARTESIAN_POINT ( 'NONE',  ( 1.321505333908973956, -3.855830693249185259, -0.03421028094655655799 ) ) ;
#23108 = CARTESIAN_POINT ( 'NONE',  ( 81.04599508018874587, -4.805938895142302769, 6.000000000000116351 ) ) ;
#23109 = DIRECTION ( 'NONE',  ( -1.000000000000000000, 4.190823558986610327E-31, -1.733449886265890494E-32 ) ) ;
#23110 = ADVANCED_FACE ( 'NONE', ( #621 ), #9557, .T. ) ;
#23111 = DIRECTION ( 'NONE',  ( -1.734723475976813750E-16, -1.000000000000000000, 3.469446951953607484E-15 ) ) ;
#23112 = VECTOR ( 'NONE', #15987, 1000.000000000000000 ) ;
#23113 = VECTOR ( 'NONE', #13905, 1000.000000000000000 ) ;
#23114 = DIRECTION ( 'NONE',  ( -6.938893903907226800E-15, 0.000000000000000000, -1.000000000000000000 ) ) ;
#23115 = CARTESIAN_POINT ( 'NONE',  ( 37.00000000000014211, 0.5000000000000004441, -9.999999999999980460 ) ) ;
#23116 = DIRECTION ( 'NONE',  ( 1.000000000000000000, 2.699383410053119644E-30, 3.330669073875432643E-16 ) ) ;
#23117 = VERTEX_POINT ( 'NONE', #2487 ) ;
#23119 = EDGE_LOOP ( 'NONE', ( #21321, #12983, #9879, #19193 ) ) ;
#23118 = ORIENTED_EDGE ( 'NONE', *, *, #13810, .F. ) ;
#23120 = VERTEX_POINT ( 'NONE', #2606 ) ;
#23122 = ORIENTED_EDGE ( 'NONE', *, *, #6032, .F. ) ;
#23121 = ORIENTED_EDGE ( 'NONE', *, *, #4458, .T. ) ;
#23123 = EDGE_LOOP ( 'NONE', ( #742, #4173, #4551, #17818 ) ) ;
#23124 = VERTEX_POINT ( 'NONE', #6262 ) ;
#23125 = CARTESIAN_POINT ( 'NONE',  ( -91.02295700146254376, -0.5000000000001045830, 6.338518968055040226 ) ) ;
#23126 = TOROIDAL_SURFACE ( 'NONE', #3587, 6.000000000000015987, 0.5000000000000000000 ) ;
#23127 = STYLED_ITEM ( 'NONE', ( #3532 ), #492 ) ;
#23128 = PLANE ( 'NONE',  #4613 ) ;
#23129 = ORIENTED_EDGE ( 'NONE', *, *, #17401, .F. ) ;
#23130 = FACE_OUTER_BOUND ( 'NONE', #1667, .T. ) ;
#23131 = DIRECTION ( 'NONE',  ( 0.000000000000000000, -1.000000000000000000, 0.000000000000000000 ) ) ;
#23132 = FACE_OUTER_BOUND ( 'NONE', #11686, .T. ) ;
#23133 = DIRECTION ( 'NONE',  ( 2.172745813409349776E-17, -1.000000000000000000, 1.309377075419428048E-16 ) ) ;
#23134 = DIRECTION ( 'NONE',  ( -3.885780586188016830E-16, -4.437342591868156373E-31, 1.000000000000000000 ) ) ;
#23135 = CARTESIAN_POINT ( 'NONE',  ( 4.000000000000004441, 0.7862748000878162502, -5.565527722372433317 ) ) ;
#23136 = DIRECTION ( 'NONE',  ( -1.333893503340774882E-15, -2.778352770573747380E-17, -1.000000000000000000 ) ) ;
#23137 = ADVANCED_FACE ( 'NONE', ( #972 ), #13550, .T. ) ;
#23138 = CARTESIAN_POINT ( 'NONE',  ( 4.071447262713884463, -2.020725942163695166, -3.500000000000000444 ) ) ;
#23139 = DIRECTION ( 'NONE',  ( 1.000000000000000000, -4.440892098500650814E-16, -7.860214984771115307E-18 ) ) ;
#23140 = CARTESIAN_POINT ( 'NONE',  ( -3.999999999708139686, 13.32455531934060744, -15.99999999999999289 ) ) ;
#23141 = CARTESIAN_POINT ( 'NONE',  ( -50.65685424949280247, -1.040834085586084257E-13, 7.500000000000062172 ) ) ;
#23142 = ORIENTED_EDGE ( 'NONE', *, *, #22798, .T. ) ;
#23143 = SHAPE_REPRESENTATION_RELATIONSHIP ( 'NONE' , 'NONE' ,  #4297, #19561 ) ;
#23144 = DIRECTION ( 'NONE',  ( 0.000000000000000000, -6.938893903907238633E-15, -1.000000000000000000 ) ) ;
#23145 = CIRCLE ( 'NONE', #15998, 2.550000000000010481 ) ;
#23146 = DIRECTION ( 'NONE',  ( 1.333893503340774882E-15, 2.778352770573747380E-17, 1.000000000000000000 ) ) ;
#23148 = VERTEX_POINT ( 'NONE', #6029 ) ;
#23147 = ORIENTED_EDGE ( 'NONE', *, *, #19473, .F. ) ;
#23149 = EDGE_CURVE ( 'NONE', #6911, #11666, #13108, .T. ) ;
#23150 = AXIS2_PLACEMENT_3D ( 'NONE', #21676, #20014, #9310 ) ;
#23151 = ORIENTED_EDGE ( 'NONE', *, *, #8934, .T. ) ;
#23152 = ORIENTED_EDGE ( 'NONE', *, *, #20317, .T. ) ;
#23153 = ORIENTED_EDGE ( 'NONE', *, *, #19503, .F. ) ;
#23154 = ORIENTED_EDGE ( 'NONE', *, *, #15102, .F. ) ;
#23155 = CARTESIAN_POINT ( 'NONE',  ( 0.000000000000000000, 2.499999999999998668, 0.000000000000000000 ) ) ;
#23156 = AXIS2_PLACEMENT_3D ( 'NONE', #19616, #8249, #23043 ) ;
#23157 = CARTESIAN_POINT ( 'NONE',  ( -2.742413778650712342, -1.325747111984083793, 4.749999999999999112 ) ) ;
#23158 = CARTESIAN_POINT ( 'NONE',  ( 4.158806965674305189, 4.075748668183988066, 0.05940377217583944769 ) ) ;
#23159 = CARTESIAN_POINT ( 'NONE',  ( 37.86602540378461157, 0.000000000000000000, -10.86602540378449255 ) ) ;
#23160 = CARTESIAN_POINT ( 'NONE',  ( 2.498001805406602216E-16, -1.291058893185205491E-15, -4.499999999999988454 ) ) ;
#23161 = CARTESIAN_POINT ( 'NONE',  ( -6.000000000000130562, 1.999999999999960032, -8.000000000000035527 ) ) ;
#23162 = DIRECTION ( 'NONE',  ( 0.000000000000000000, 0.000000000000000000, -1.000000000000000000 ) ) ;
#23163 = CARTESIAN_POINT ( 'NONE',  ( 7.499999999999978684, -8.000000000000051514, 6.249999999999977796 ) ) ;
#23164 = DIRECTION ( 'NONE',  ( 0.000000000000000000, 0.000000000000000000, -1.000000000000000000 ) ) ;
#23165 = DIRECTION ( 'NONE',  ( -1.000000000000000000, 0.000000000000000000, 0.000000000000000000 ) ) ;
#23166 = AXIS2_PLACEMENT_3D ( 'NONE', #1749, #8700, #23068 ) ;
#23167 = DIRECTION ( 'NONE',  ( 3.330669073875457788E-16, 0.000000000000000000, -1.000000000000000000 ) ) ;
#23168 = DIRECTION ( 'NONE',  ( 0.000000000000000000, 0.000000000000000000, -1.000000000000000000 ) ) ;
#23169 = CARTESIAN_POINT ( 'NONE',  ( -0.6640947660583549350, 4.471078309994097388, -3.602146406945683221 ) ) ;
#23170 = AXIS2_PLACEMENT_3D ( 'NONE', #3731, #1398, #8573 ) ;
#23171 = EDGE_CURVE ( 'NONE', #16292, #1099, #13321, .T. ) ;
#23172 = CYLINDRICAL_SURFACE ( 'NONE', #18740, 0.2500000000000003331 ) ;
#23173 = CARTESIAN_POINT ( 'NONE',  ( 4.086262841041386373, 2.102637316508701559, -3.500000000000009326 ) ) ;
#23174 = ORIENTED_EDGE ( 'NONE', *, *, #4481, .T. ) ;
#23175 = ADVANCED_FACE ( 'NONE', ( #22495 ), #7786, .T. ) ;
#23176 = VERTEX_POINT ( 'NONE', #6147 ) ;
#23177 = CARTESIAN_POINT ( 'NONE',  ( 0.000000000000000000, -3.031088913245536087, -1.749999999999996447 ) ) ;
#23180 = ORIENTED_EDGE ( 'NONE', *, *, #7304, .F. ) ;
#23179 = EDGE_CURVE ( 'NONE', #17819, #6667, #9192, .T. ) ;
#23178 = EDGE_LOOP ( 'NONE', ( #19953, #17417, #8699, #19598 ) ) ;
#23181 = FACE_OUTER_BOUND ( 'NONE', #2033, .T. ) ;
#23182 = EDGE_CURVE ( 'NONE', #22005, #14576, #18837, .T. ) ;
#23183 = CARTESIAN_POINT ( 'NONE',  ( 2.345747346278090451, -3.264484291692558937, -0.01223254789877006345 ) ) ;
#23184 = CARTESIAN_POINT ( 'NONE',  ( 114.8016533820240568, -5.880524088665878502, -6.499999999999970690 ) ) ;
#23185 = VECTOR ( 'NONE', #5946, 1000.000000000000000 ) ;
#23186 = ORIENTED_EDGE ( 'NONE', *, *, #11079, .T. ) ;
#23187 = CARTESIAN_POINT ( 'NONE',  ( -67.28510754798028870, 3.200000000000022382, 12.22107821754958579 ) ) ;
#23188 = CARTESIAN_POINT ( 'NONE',  ( -42.54314575050796776, 3.999999999999996447, -8.000000000000035527 ) ) ;
#23189 = DIRECTION ( 'NONE',  ( 0.000000000000000000, -0.000000000000000000, 1.000000000000000000 ) ) ;
#23190 = CARTESIAN_POINT ( 'NONE',  ( 3.999999999999989786, -2.309401076758549998, -0.3572655899081733644 ) ) ;
#23191 = DIRECTION ( 'NONE',  ( 0.000000000000000000, 0.000000000000000000, 1.000000000000000000 ) ) ;
#23192 = CARTESIAN_POINT ( 'NONE',  ( 3.999999999999948042, 2.309401076758532678, -3.433295621305378020 ) ) ;
#23193 = LINE ( 'NONE', #21197, #3498 ) ;
#23194 = CARTESIAN_POINT ( 'NONE',  ( 4.033901012036468892, -3.740908793663292098, 0.5205559028931424637 ) ) ;
#23195 = EDGE_CURVE ( 'NONE', #19862, #8293, #17178, .T. ) ;
#23196 = EDGE_CURVE ( 'NONE', #17995, #2357, #19845, .T. ) ;
#23197 = VECTOR ( 'NONE', #3331, 1000.000000000000227 ) ;
#23198 = B_SPLINE_CURVE_WITH_KNOTS ( 'NONE', 3,
 ( #14615, #3901, #2023, #13081, #5808, #505 ),
 .UNSPECIFIED., .F., .F.,
 ( 4, 2, 4 ),
 ( 0.000000000000000000, 0.002086519881787257148, 0.004173039763574514296 ),
 .UNSPECIFIED. ) ;
#23199 = FACE_OUTER_BOUND ( 'NONE', #954, .T. ) ;
#23200 = CARTESIAN_POINT ( 'NONE',  ( -2.428612866367529932E-14, 4.250000000000003553, -17.75000000000000711 ) ) ;
#23201 = VERTEX_POINT ( 'NONE', #13669 ) ;
#23202 = AXIS2_PLACEMENT_3D ( 'NONE', #20619, #8139, #2844 ) ;
#23203 = EDGE_CURVE ( 'NONE', #13382, #6061, #6332, .T. ) ;
#23204 = SHAPE_DEFINITION_REPRESENTATION ( #6671, #17992 ) ;
#23206 = ORIENTED_EDGE ( 'NONE', *, *, #22120, .T. ) ;
#23205 = ORIENTED_EDGE ( 'NONE', *, *, #2180, .T. ) ;
#23207 = ORIENTED_EDGE ( 'NONE', *, *, #13742, .F. ) ;
#23208 = CIRCLE ( 'NONE', #20948, 6.999999999999999112 ) ;
#23211 = ORIENTED_EDGE ( 'NONE', *, *, #8790, .T. ) ;
#23210 = EDGE_CURVE ( 'NONE', #21722, #6874, #17212, .T. ) ;
#23209 = ORIENTED_EDGE ( 'NONE', *, *, #16619, .T. ) ;
#23212 = LINE ( 'NONE', #22972, #15149 ) ;
#23213 = FACE_BOUND ( 'NONE', #21957, .T. ) ;
#23214 = DIRECTION ( 'NONE',  ( -3.885780586188016830E-16, -4.437342591868156373E-31, 1.000000000000000000 ) ) ;
#23215 = DIRECTION ( 'NONE',  ( 4.615739097524201565E-16, 1.000000000000000000, 1.224646799147356905E-16 ) ) ;
#23216 = CARTESIAN_POINT ( 'NONE',  ( 12.84999999999997300, -1.499999999999997780, 1.387778780781445676E-14 ) ) ;
#23217 = VECTOR ( 'NONE', #17767, 1000.000000000000000 ) ;
#23218 = DIRECTION ( 'NONE',  ( -0.000000000000000000, -0.000000000000000000, -1.000000000000000000 ) ) ;
#23219 = CARTESIAN_POINT ( 'NONE',  ( 110.9706201109471522, -9.453020409440348715, 6.000000000000088818 ) ) ;
#23220 = AXIS2_PLACEMENT_3D ( 'NONE', #14309, #21138, #10769 ) ;
#23221 = CARTESIAN_POINT ( 'NONE',  ( -91.02295700146257218, -3.200000000000101874, 6.338518968055012692 ) ) ;
#23222 = FACE_OUTER_BOUND ( 'NONE', #19488, .T. ) ;
#23223 = DIRECTION ( 'NONE',  ( -0.8571428571428568732, 7.888609052210126812E-31, -0.5150787536377133824 ) ) ;
#23224 = APPLICATION_CONTEXT ( 'automotive_design' ) ;
#23225 = EDGE_CURVE ( 'NONE', #10857, #7917, #4242, .T. ) ;
#23226 = CARTESIAN_POINT ( 'NONE',  ( 119.5756419024615269, -4.500000000000059508, -5.999999999999984901 ) ) ;
#23227 = EDGE_CURVE ( 'NONE', #6061, #16716, #21377, .T. ) ;
#23228 = CARTESIAN_POINT ( 'NONE',  ( 116.5066492821803195, -7.708908342713815642, -5.999999999999998224 ) ) ;
#23229 = CIRCLE ( 'NONE', #1412, 6.500000000000005329 ) ;
#23230 = ADVANCED_FACE ( 'NONE', ( #1094 ), #15417, .F. ) ;
#23231 = CARTESIAN_POINT ( 'NONE',  ( 63.50658097017372938, -7.000000000000006217, 6.500000000000068390 ) ) ;
#23232 = CARTESIAN_POINT ( 'NONE',  ( -6.000000000000019540, -8.000000000000042633, 7.500000000000062172 ) ) ;
#23233 = CARTESIAN_POINT ( 'NONE',  ( 4.033901012035799205, -3.740908793663177523, 0.5205559028926609599 ) ) ;
#23234 = PRODUCT ( 'hex flange bolt small_iso_ISO 4162 - M5 x 20 x 20-N', 'hex flange bolt small_iso_ISO 4162 - M5 x 20 x 20-N', '', ( #20245 ) ) ;
#23235 = VERTEX_POINT ( 'NONE', #11890 ) ;
#23236 = AXIS2_PLACEMENT_3D ( 'NONE', #15960, #5276, #23165 ) ;
#23238 = ORIENTED_EDGE ( 'NONE', *, *, #2439, .F. ) ;
#23237 = ORIENTED_EDGE ( 'NONE', *, *, #19604, .T. ) ;
#23239 = EDGE_CURVE ( 'NONE', #2560, #3580, #10851, .T. ) ;
#23240 = ORIENTED_EDGE ( 'NONE', *, *, #22798, .F. ) ;
#23242 = ORIENTED_EDGE ( 'NONE', *, *, #16873, .T. ) ;
#23241 = ORIENTED_EDGE ( 'NONE', *, *, #11679, .T. ) ;
#23243 = VERTEX_POINT ( 'NONE', #15062 ) ;
#23244 = EDGE_LOOP ( 'NONE', ( #4948, #14387, #17844, #21593 ) ) ;
#23245 = EDGE_LOOP ( 'NONE', ( #2671, #11183, #510, #14513 ) ) ;
#23246 = DIRECTION ( 'NONE',  ( -5.004010026856173173E-16, -1.201780285297635391E-31, 1.000000000000000000 ) ) ;
#23247 = VECTOR ( 'NONE', #19186, 1000.000000000000000 ) ;
#23248 = AXIS2_PLACEMENT_3D ( 'NONE', #11591, #4534, #907 ) ;
#23249 = DIRECTION ( 'NONE',  ( -1.000000000000000000, 4.190823558986610327E-31, -1.733449886265890494E-32 ) ) ;
#23250 = CARTESIAN_POINT ( 'NONE',  ( -7.607945571813328201, -13.10245601331111587, 8.443122311927368173 ) ) ;
#23251 = DIRECTION ( 'NONE',  ( 0.000000000000000000, 0.7453559924999302311, 0.6666666666666662966 ) ) ;
#23252 = CARTESIAN_POINT ( 'NONE',  ( 57.49335071782242323, -0.7089083427137543580, -6.499999999999922728 ) ) ;
#23253 = CARTESIAN_POINT ( 'NONE',  ( 124.5000000000019185, -7.000000000000062172, -5.999999999999984901 ) ) ;
#23254 = DIRECTION ( 'NONE',  ( 0.000000000000000000, 0.000000000000000000, -1.000000000000000000 ) ) ;
#23255 = SURFACE_STYLE_FILL_AREA ( #10986 ) ;
#23256 = COLOUR_RGB ( '', 0.09019608, 0.27058824, 0.51372549) ;
#23257 = DIRECTION ( 'NONE',  ( 2.220446049250313081E-16, -1.000000000000000000, 7.025792437124636392E-31 ) ) ;
#23258 = CARTESIAN_POINT ( 'NONE',  ( 0.000000000000000000, -3.031088913245536087, -1.750000000000001554 ) ) ;
#23259 = CARTESIAN_POINT ( 'NONE',  ( -6.683546854663853232, 13.99327871316343952, -17.64411577037000356 ) ) ;
#23260 = FACE_OUTER_BOUND ( 'NONE', #4260, .T. ) ;
#23261 = ORIENTED_EDGE ( 'NONE', *, *, #15752, .T. ) ;
#23262 = TOROIDAL_SURFACE ( 'NONE', #16087, 4.500000000000002665, 0.5000000000000000000 ) ;
#23263 = CARTESIAN_POINT ( 'NONE',  ( 0.000000000000000000, -1.750000000000001554, 0.000000000000000000 ) ) ;
#23264 = DIRECTION ( 'NONE',  ( 0.000000000000000000, 0.000000000000000000, 1.000000000000000000 ) ) ;
#23265 = AXIS2_PLACEMENT_3D ( 'NONE', #14414, #6767, #13935 ) ;
#23267 = ORIENTED_EDGE ( 'NONE', *, *, #6362, .T. ) ;
#23266 = ORIENTED_EDGE ( 'NONE', *, *, #16432, .T. ) ;
#23268 = CARTESIAN_POINT ( 'NONE',  ( -4.236525694536651621, 2.416953475386471872, -3.751298745799860335 ) ) ;
#23269 = NEXT_ASSEMBLY_USAGE_OCCURRENCE ( 'NAUO1', ' ', ' ', #11778, #22880, $ ) ;
#23270 = NEXT_ASSEMBLY_USAGE_OCCURRENCE ( 'NAUO2', ' ', ' ', #11778, #17672, $ ) ;
#23271 = NEXT_ASSEMBLY_USAGE_OCCURRENCE ( 'NAUO3', ' ', ' ', #11778, #17672, $ ) ;
#23272 = NEXT_ASSEMBLY_USAGE_OCCURRENCE ( 'NAUO4', ' ', ' ', #11778, #11058, $ ) ;
#23273 = NEXT_ASSEMBLY_USAGE_OCCURRENCE ( 'NAUO5', ' ', ' ', #11778, #18401, $ ) ;
#23274 = NEXT_ASSEMBLY_USAGE_OCCURRENCE ( 'NAUO6', ' ', ' ', #11778, #15220, $ ) ;
#23275 = NEXT_ASSEMBLY_USAGE_OCCURRENCE ( 'NAUO7', ' ', ' ', #11778, #21853, $ ) ;
#23276 = NEXT_ASSEMBLY_USAGE_OCCURRENCE ( 'NAUO8', ' ', ' ', #11778, #4448, $ ) ;
#23277 = NEXT_ASSEMBLY_USAGE_OCCURRENCE ( 'NAUO9', ' ', ' ', #11778, #9348, $ ) ;
#23278 = NEXT_ASSEMBLY_USAGE_OCCURRENCE ( 'NAUO10', ' ', ' ', #11778, #4448, $ ) ;
#23279 = NEXT_ASSEMBLY_USAGE_OCCURRENCE ( 'NAUO11', ' ', ' ', #11778, #8624, $ ) ;
#23280 = NEXT_ASSEMBLY_USAGE_OCCURRENCE ( 'NAUO12', ' ', ' ', #11778, #21145, $ ) ;
#23281 = NEXT_ASSEMBLY_USAGE_OCCURRENCE ( 'NAUO13', ' ', ' ', #11778, #20122, $ ) ;
#23282 = NEXT_ASSEMBLY_USAGE_OCCURRENCE ( 'NAUO14', ' ', ' ', #11778, #7617, $ ) ;
#23283 = NEXT_ASSEMBLY_USAGE_OCCURRENCE ( 'NAUO15', ' ', ' ', #11778, #2001, $ ) ;
#23284 = NEXT_ASSEMBLY_USAGE_OCCURRENCE ( 'NAUO16', ' ', ' ', #11778, #3448, $ ) ;
#23285 = NEXT_ASSEMBLY_USAGE_OCCURRENCE ( 'NAUO17', ' ', ' ', #11778, #14519, $ ) ;
#23286 = NEXT_ASSEMBLY_USAGE_OCCURRENCE ( 'NAUO18', ' ', ' ', #11778, #14519, $ ) ;
#23287 = NEXT_ASSEMBLY_USAGE_OCCURRENCE ( 'NAUO19', ' ', ' ', #11778, #20858, $ ) ;
#23288 = NEXT_ASSEMBLY_USAGE_OCCURRENCE ( 'NAUO20', ' ', ' ', #11778, #20858, $ ) ;
ENDSEC;
END-ISO-10303-21;
